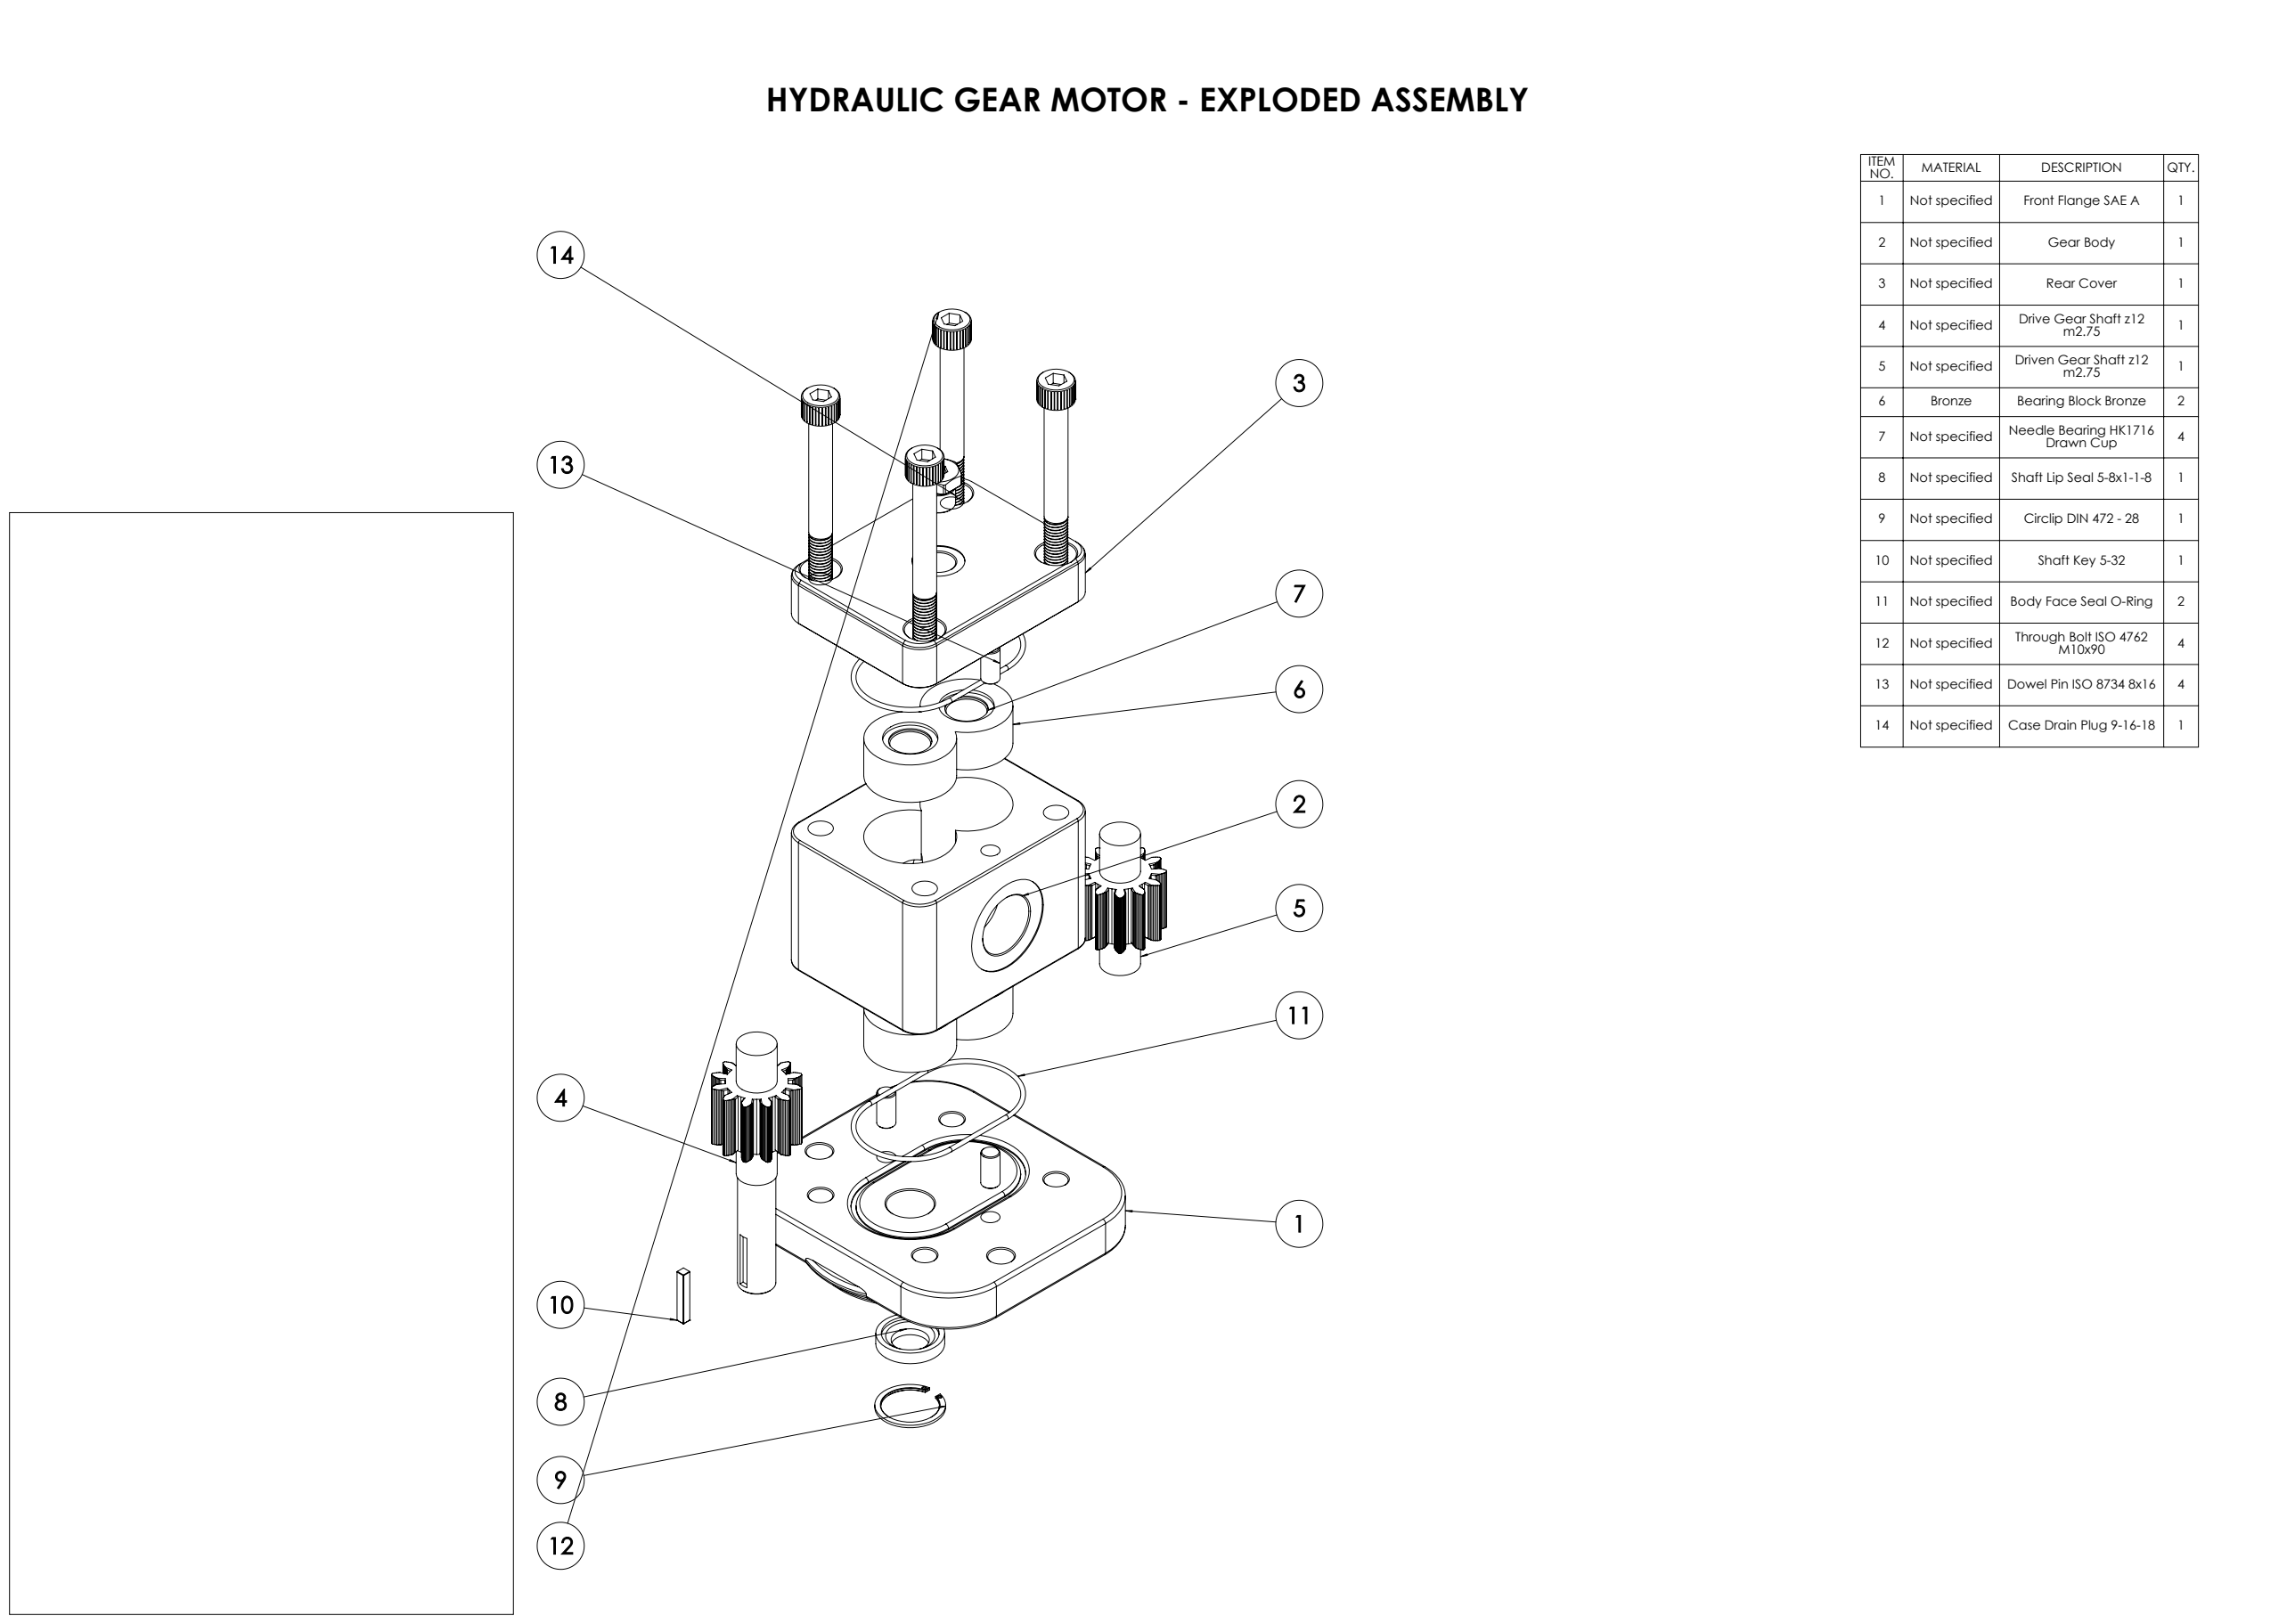
ISO-10303-21;
HEADER;
/* Generated by software containing ST-Developer
 * from STEP Tools, Inc. (www.steptools.com) 
 */

FILE_DESCRIPTION(
/* description */ (''),
/* implementation_level */ '2;1');

FILE_NAME(
/* name */ 'MAS-346',
/* time_stamp */ '2026-10-26T06:59:52-07:00',
/* author */ (''),
/* organization */ (''),
/* preprocessor_version */ 'ST-DEVELOPER v20.2',
/* originating_system */ 'Autodesk Translation Framework v15.15.0.0',
/* authorisation */ '');

FILE_SCHEMA (('AUTOMOTIVE_DESIGN { 1 0 10303 214 3 1 1 }'));
ENDSEC;

DATA;
#10=MECHANICAL_DESIGN_GEOMETRIC_PRESENTATION_REPRESENTATION('',(#164,#165,
#166,#167,#168,#169,#170,#171,#172,#173,#174,#175,#176,#177),#46395);
#11=ITEM_DEFINED_TRANSFORMATION($,$,#25107,#26908);
#12=ITEM_DEFINED_TRANSFORMATION($,$,#25445,#26909);
#13=ITEM_DEFINED_TRANSFORMATION($,$,#25562,#26910);
#14=ITEM_DEFINED_TRANSFORMATION($,$,#25703,#26911);
#15=ITEM_DEFINED_TRANSFORMATION($,$,#26063,#26912);
#16=ITEM_DEFINED_TRANSFORMATION($,$,#26410,#26913);
#17=ITEM_DEFINED_TRANSFORMATION($,$,#26410,#26914);
#18=ITEM_DEFINED_TRANSFORMATION($,$,#26435,#26915);
#19=ITEM_DEFINED_TRANSFORMATION($,$,#26457,#26916);
#20=ITEM_DEFINED_TRANSFORMATION($,$,#26494,#26917);
#21=ITEM_DEFINED_TRANSFORMATION($,$,#26513,#26918);
#22=ITEM_DEFINED_TRANSFORMATION($,$,#26513,#26919);
#23=ITEM_DEFINED_TRANSFORMATION($,$,#26528,#26920);
#24=ITEM_DEFINED_TRANSFORMATION($,$,#26580,#26921);
#25=ITEM_DEFINED_TRANSFORMATION($,$,#26580,#26922);
#26=ITEM_DEFINED_TRANSFORMATION($,$,#26580,#26923);
#27=ITEM_DEFINED_TRANSFORMATION($,$,#26580,#26924);
#28=ITEM_DEFINED_TRANSFORMATION($,$,#26605,#26925);
#29=ITEM_DEFINED_TRANSFORMATION($,$,#26605,#26926);
#30=ITEM_DEFINED_TRANSFORMATION($,$,#26605,#26927);
#31=ITEM_DEFINED_TRANSFORMATION($,$,#26605,#26928);
#32=ITEM_DEFINED_TRANSFORMATION($,$,#26898,#26929);
#33=ITEM_DEFINED_TRANSFORMATION($,$,#26898,#26930);
#34=ITEM_DEFINED_TRANSFORMATION($,$,#26898,#26931);
#35=ITEM_DEFINED_TRANSFORMATION($,$,#26898,#26932);
#36=(
REPRESENTATION_RELATIONSHIP($,$,#46456,#46455)
REPRESENTATION_RELATIONSHIP_WITH_TRANSFORMATION(#11)
SHAPE_REPRESENTATION_RELATIONSHIP()
);
#37=(
REPRESENTATION_RELATIONSHIP($,$,#46457,#46455)
REPRESENTATION_RELATIONSHIP_WITH_TRANSFORMATION(#12)
SHAPE_REPRESENTATION_RELATIONSHIP()
);
#38=(
REPRESENTATION_RELATIONSHIP($,$,#46458,#46455)
REPRESENTATION_RELATIONSHIP_WITH_TRANSFORMATION(#13)
SHAPE_REPRESENTATION_RELATIONSHIP()
);
#39=(
REPRESENTATION_RELATIONSHIP($,$,#46459,#46455)
REPRESENTATION_RELATIONSHIP_WITH_TRANSFORMATION(#14)
SHAPE_REPRESENTATION_RELATIONSHIP()
);
#40=(
REPRESENTATION_RELATIONSHIP($,$,#46460,#46455)
REPRESENTATION_RELATIONSHIP_WITH_TRANSFORMATION(#15)
SHAPE_REPRESENTATION_RELATIONSHIP()
);
#41=(
REPRESENTATION_RELATIONSHIP($,$,#46461,#46455)
REPRESENTATION_RELATIONSHIP_WITH_TRANSFORMATION(#16)
SHAPE_REPRESENTATION_RELATIONSHIP()
);
#42=(
REPRESENTATION_RELATIONSHIP($,$,#46461,#46455)
REPRESENTATION_RELATIONSHIP_WITH_TRANSFORMATION(#17)
SHAPE_REPRESENTATION_RELATIONSHIP()
);
#43=(
REPRESENTATION_RELATIONSHIP($,$,#46462,#46455)
REPRESENTATION_RELATIONSHIP_WITH_TRANSFORMATION(#18)
SHAPE_REPRESENTATION_RELATIONSHIP()
);
#44=(
REPRESENTATION_RELATIONSHIP($,$,#46463,#46455)
REPRESENTATION_RELATIONSHIP_WITH_TRANSFORMATION(#19)
SHAPE_REPRESENTATION_RELATIONSHIP()
);
#45=(
REPRESENTATION_RELATIONSHIP($,$,#46464,#46455)
REPRESENTATION_RELATIONSHIP_WITH_TRANSFORMATION(#20)
SHAPE_REPRESENTATION_RELATIONSHIP()
);
#46=(
REPRESENTATION_RELATIONSHIP($,$,#46465,#46455)
REPRESENTATION_RELATIONSHIP_WITH_TRANSFORMATION(#21)
SHAPE_REPRESENTATION_RELATIONSHIP()
);
#47=(
REPRESENTATION_RELATIONSHIP($,$,#46465,#46455)
REPRESENTATION_RELATIONSHIP_WITH_TRANSFORMATION(#22)
SHAPE_REPRESENTATION_RELATIONSHIP()
);
#48=(
REPRESENTATION_RELATIONSHIP($,$,#46466,#46455)
REPRESENTATION_RELATIONSHIP_WITH_TRANSFORMATION(#23)
SHAPE_REPRESENTATION_RELATIONSHIP()
);
#49=(
REPRESENTATION_RELATIONSHIP($,$,#46467,#46455)
REPRESENTATION_RELATIONSHIP_WITH_TRANSFORMATION(#24)
SHAPE_REPRESENTATION_RELATIONSHIP()
);
#50=(
REPRESENTATION_RELATIONSHIP($,$,#46467,#46455)
REPRESENTATION_RELATIONSHIP_WITH_TRANSFORMATION(#25)
SHAPE_REPRESENTATION_RELATIONSHIP()
);
#51=(
REPRESENTATION_RELATIONSHIP($,$,#46467,#46455)
REPRESENTATION_RELATIONSHIP_WITH_TRANSFORMATION(#26)
SHAPE_REPRESENTATION_RELATIONSHIP()
);
#52=(
REPRESENTATION_RELATIONSHIP($,$,#46467,#46455)
REPRESENTATION_RELATIONSHIP_WITH_TRANSFORMATION(#27)
SHAPE_REPRESENTATION_RELATIONSHIP()
);
#53=(
REPRESENTATION_RELATIONSHIP($,$,#46468,#46455)
REPRESENTATION_RELATIONSHIP_WITH_TRANSFORMATION(#28)
SHAPE_REPRESENTATION_RELATIONSHIP()
);
#54=(
REPRESENTATION_RELATIONSHIP($,$,#46468,#46455)
REPRESENTATION_RELATIONSHIP_WITH_TRANSFORMATION(#29)
SHAPE_REPRESENTATION_RELATIONSHIP()
);
#55=(
REPRESENTATION_RELATIONSHIP($,$,#46468,#46455)
REPRESENTATION_RELATIONSHIP_WITH_TRANSFORMATION(#30)
SHAPE_REPRESENTATION_RELATIONSHIP()
);
#56=(
REPRESENTATION_RELATIONSHIP($,$,#46468,#46455)
REPRESENTATION_RELATIONSHIP_WITH_TRANSFORMATION(#31)
SHAPE_REPRESENTATION_RELATIONSHIP()
);
#57=(
REPRESENTATION_RELATIONSHIP($,$,#46469,#46455)
REPRESENTATION_RELATIONSHIP_WITH_TRANSFORMATION(#32)
SHAPE_REPRESENTATION_RELATIONSHIP()
);
#58=(
REPRESENTATION_RELATIONSHIP($,$,#46469,#46455)
REPRESENTATION_RELATIONSHIP_WITH_TRANSFORMATION(#33)
SHAPE_REPRESENTATION_RELATIONSHIP()
);
#59=(
REPRESENTATION_RELATIONSHIP($,$,#46469,#46455)
REPRESENTATION_RELATIONSHIP_WITH_TRANSFORMATION(#34)
SHAPE_REPRESENTATION_RELATIONSHIP()
);
#60=(
REPRESENTATION_RELATIONSHIP($,$,#46469,#46455)
REPRESENTATION_RELATIONSHIP_WITH_TRANSFORMATION(#35)
SHAPE_REPRESENTATION_RELATIONSHIP()
);
#61=CONTEXT_DEPENDENT_SHAPE_REPRESENTATION(#36,#46430);
#62=CONTEXT_DEPENDENT_SHAPE_REPRESENTATION(#37,#46431);
#63=CONTEXT_DEPENDENT_SHAPE_REPRESENTATION(#38,#46432);
#64=CONTEXT_DEPENDENT_SHAPE_REPRESENTATION(#39,#46433);
#65=CONTEXT_DEPENDENT_SHAPE_REPRESENTATION(#40,#46434);
#66=CONTEXT_DEPENDENT_SHAPE_REPRESENTATION(#41,#46435);
#67=CONTEXT_DEPENDENT_SHAPE_REPRESENTATION(#42,#46436);
#68=CONTEXT_DEPENDENT_SHAPE_REPRESENTATION(#43,#46437);
#69=CONTEXT_DEPENDENT_SHAPE_REPRESENTATION(#44,#46438);
#70=CONTEXT_DEPENDENT_SHAPE_REPRESENTATION(#45,#46439);
#71=CONTEXT_DEPENDENT_SHAPE_REPRESENTATION(#46,#46440);
#72=CONTEXT_DEPENDENT_SHAPE_REPRESENTATION(#47,#46441);
#73=CONTEXT_DEPENDENT_SHAPE_REPRESENTATION(#48,#46442);
#74=CONTEXT_DEPENDENT_SHAPE_REPRESENTATION(#49,#46443);
#75=CONTEXT_DEPENDENT_SHAPE_REPRESENTATION(#50,#46444);
#76=CONTEXT_DEPENDENT_SHAPE_REPRESENTATION(#51,#46445);
#77=CONTEXT_DEPENDENT_SHAPE_REPRESENTATION(#52,#46446);
#78=CONTEXT_DEPENDENT_SHAPE_REPRESENTATION(#53,#46447);
#79=CONTEXT_DEPENDENT_SHAPE_REPRESENTATION(#54,#46448);
#80=CONTEXT_DEPENDENT_SHAPE_REPRESENTATION(#55,#46449);
#81=CONTEXT_DEPENDENT_SHAPE_REPRESENTATION(#56,#46450);
#82=CONTEXT_DEPENDENT_SHAPE_REPRESENTATION(#57,#46451);
#83=CONTEXT_DEPENDENT_SHAPE_REPRESENTATION(#58,#46452);
#84=CONTEXT_DEPENDENT_SHAPE_REPRESENTATION(#59,#46453);
#85=CONTEXT_DEPENDENT_SHAPE_REPRESENTATION(#60,#46454);
#86=NEXT_ASSEMBLY_USAGE_OCCURRENCE('01_Front_Flange_SAE_A:2',
'01_Front_Flange_SAE_A:2','01_Front_Flange_SAE_A:2',#46471,#46472,
'01_Front_Flange_SAE_A:2');
#87=NEXT_ASSEMBLY_USAGE_OCCURRENCE('02_Gear_Body:2','02_Gear_Body:2',
'02_Gear_Body:2',#46471,#46473,'02_Gear_Body:2');
#88=NEXT_ASSEMBLY_USAGE_OCCURRENCE('03_Rear_Cover:2','03_Rear_Cover:2',
'03_Rear_Cover:2',#46471,#46474,'03_Rear_Cover:2');
#89=NEXT_ASSEMBLY_USAGE_OCCURRENCE('04_Drive_Gear_Shaft_z12_m2.75:2',
'04_Drive_Gear_Shaft_z12_m2.75:2','04_Drive_Gear_Shaft_z12_m2.75:2',#46471,
#46475,'04_Drive_Gear_Shaft_z12_m2.75:2');
#90=NEXT_ASSEMBLY_USAGE_OCCURRENCE('05_Driven_Gear_Shaft_z12_m2.75:2',
'05_Driven_Gear_Shaft_z12_m2.75:2','05_Driven_Gear_Shaft_z12_m2.75:2',#46471,
#46476,'05_Driven_Gear_Shaft_z12_m2.75:2');
#91=NEXT_ASSEMBLY_USAGE_OCCURRENCE('06_Bearing_Block_Bronze:2',
'06_Bearing_Block_Bronze:2','06_Bearing_Block_Bronze:2',#46471,#46477,
'06_Bearing_Block_Bronze:2');
#92=NEXT_ASSEMBLY_USAGE_OCCURRENCE('06_Bearing_Block_Bronze:3',
'06_Bearing_Block_Bronze:3','06_Bearing_Block_Bronze:3',#46471,#46477,
'06_Bearing_Block_Bronze:3');
#93=NEXT_ASSEMBLY_USAGE_OCCURRENCE('08_Shaft_Lip_Seal_5-8x1-1-8:2',
'08_Shaft_Lip_Seal_5-8x1-1-8:2','08_Shaft_Lip_Seal_5-8x1-1-8:2',#46471,
#46478,'08_Shaft_Lip_Seal_5-8x1-1-8:2');
#94=NEXT_ASSEMBLY_USAGE_OCCURRENCE('09_Circlip_DIN_472_-_28:2',
'09_Circlip_DIN_472_-_28:2','09_Circlip_DIN_472_-_28:2',#46471,#46479,
'09_Circlip_DIN_472_-_28:2');
#95=NEXT_ASSEMBLY_USAGE_OCCURRENCE('10_Shaft_Key_5-32:2',
'10_Shaft_Key_5-32:2','10_Shaft_Key_5-32:2',#46471,#46480,
'10_Shaft_Key_5-32:2');
#96=NEXT_ASSEMBLY_USAGE_OCCURRENCE('11_Body_Face_Seal_O-Ring:2',
'11_Body_Face_Seal_O-Ring:2','11_Body_Face_Seal_O-Ring:2',#46471,#46481,
'11_Body_Face_Seal_O-Ring:2');
#97=NEXT_ASSEMBLY_USAGE_OCCURRENCE('11_Body_Face_Seal_O-Ring:3',
'11_Body_Face_Seal_O-Ring:3','11_Body_Face_Seal_O-Ring:3',#46471,#46481,
'11_Body_Face_Seal_O-Ring:3');
#98=NEXT_ASSEMBLY_USAGE_OCCURRENCE('14_Case_Drain_Plug_9-16-18:2',
'14_Case_Drain_Plug_9-16-18:2','14_Case_Drain_Plug_9-16-18:2',#46471,#46482,
'14_Case_Drain_Plug_9-16-18:2');
#99=NEXT_ASSEMBLY_USAGE_OCCURRENCE(
'07_Needle_Bearing_HK1716_Drawn_Cup:2',
'07_Needle_Bearing_HK1716_Drawn_Cup:2',
'07_Needle_Bearing_HK1716_Drawn_Cup:2',#46471,#46483,
'07_Needle_Bearing_HK1716_Drawn_Cup:2');
#100=NEXT_ASSEMBLY_USAGE_OCCURRENCE(
'07_Needle_Bearing_HK1716_Drawn_Cup:3',
'07_Needle_Bearing_HK1716_Drawn_Cup:3',
'07_Needle_Bearing_HK1716_Drawn_Cup:3',#46471,#46483,
'07_Needle_Bearing_HK1716_Drawn_Cup:3');
#101=NEXT_ASSEMBLY_USAGE_OCCURRENCE(
'07_Needle_Bearing_HK1716_Drawn_Cup:4',
'07_Needle_Bearing_HK1716_Drawn_Cup:4',
'07_Needle_Bearing_HK1716_Drawn_Cup:4',#46471,#46483,
'07_Needle_Bearing_HK1716_Drawn_Cup:4');
#102=NEXT_ASSEMBLY_USAGE_OCCURRENCE(
'07_Needle_Bearing_HK1716_Drawn_Cup:5',
'07_Needle_Bearing_HK1716_Drawn_Cup:5',
'07_Needle_Bearing_HK1716_Drawn_Cup:5',#46471,#46483,
'07_Needle_Bearing_HK1716_Drawn_Cup:5');
#103=NEXT_ASSEMBLY_USAGE_OCCURRENCE('12_Through_Bolt_ISO_4762_M10x90:2',
'12_Through_Bolt_ISO_4762_M10x90:2','12_Through_Bolt_ISO_4762_M10x90:2',
#46471,#46484,'12_Through_Bolt_ISO_4762_M10x90:2');
#104=NEXT_ASSEMBLY_USAGE_OCCURRENCE('12_Through_Bolt_ISO_4762_M10x90:3',
'12_Through_Bolt_ISO_4762_M10x90:3','12_Through_Bolt_ISO_4762_M10x90:3',
#46471,#46484,'12_Through_Bolt_ISO_4762_M10x90:3');
#105=NEXT_ASSEMBLY_USAGE_OCCURRENCE('12_Through_Bolt_ISO_4762_M10x90:4',
'12_Through_Bolt_ISO_4762_M10x90:4','12_Through_Bolt_ISO_4762_M10x90:4',
#46471,#46484,'12_Through_Bolt_ISO_4762_M10x90:4');
#106=NEXT_ASSEMBLY_USAGE_OCCURRENCE('12_Through_Bolt_ISO_4762_M10x90:5',
'12_Through_Bolt_ISO_4762_M10x90:5','12_Through_Bolt_ISO_4762_M10x90:5',
#46471,#46484,'12_Through_Bolt_ISO_4762_M10x90:5');
#107=NEXT_ASSEMBLY_USAGE_OCCURRENCE('13_Dowel_Pin_ISO_8734_8x16:2',
'13_Dowel_Pin_ISO_8734_8x16:2','13_Dowel_Pin_ISO_8734_8x16:2',#46471,#46485,
'13_Dowel_Pin_ISO_8734_8x16:2');
#108=NEXT_ASSEMBLY_USAGE_OCCURRENCE('13_Dowel_Pin_ISO_8734_8x16:3',
'13_Dowel_Pin_ISO_8734_8x16:3','13_Dowel_Pin_ISO_8734_8x16:3',#46471,#46485,
'13_Dowel_Pin_ISO_8734_8x16:3');
#109=NEXT_ASSEMBLY_USAGE_OCCURRENCE('13_Dowel_Pin_ISO_8734_8x16:4',
'13_Dowel_Pin_ISO_8734_8x16:4','13_Dowel_Pin_ISO_8734_8x16:4',#46471,#46485,
'13_Dowel_Pin_ISO_8734_8x16:4');
#110=NEXT_ASSEMBLY_USAGE_OCCURRENCE('13_Dowel_Pin_ISO_8734_8x16:5',
'13_Dowel_Pin_ISO_8734_8x16:5','13_Dowel_Pin_ISO_8734_8x16:5',#46471,#46485,
'13_Dowel_Pin_ISO_8734_8x16:5');
#111=ELLIPSE('',#26459,20.7889393668845,14.7);
#112=ELLIPSE('',#26464,20.7889393668845,14.7);
#113=ELLIPSE('',#26470,20.7889393668845,14.7);
#114=ELLIPSE('',#26474,20.7889393668845,14.7);
#115=(
BOUNDED_CURVE()
B_SPLINE_CURVE(2,(#35773,#35774,#35775),.UNSPECIFIED.,.F.,.F.)
B_SPLINE_CURVE_WITH_KNOTS((3,3),(0.,0.297909382195316),.UNSPECIFIED.)
CURVE()
GEOMETRIC_REPRESENTATION_ITEM()
RATIONAL_B_SPLINE_CURVE((1.,1.,1.))
REPRESENTATION_ITEM('')
);
#116=(
BOUNDED_CURVE()
B_SPLINE_CURVE(2,(#35780,#35781,#35782),.UNSPECIFIED.,.F.,.F.)
B_SPLINE_CURVE_WITH_KNOTS((3,3),(0.297909382195316,0.595818764390632),
 .UNSPECIFIED.)
CURVE()
GEOMETRIC_REPRESENTATION_ITEM()
RATIONAL_B_SPLINE_CURVE((1.,1.,1.))
REPRESENTATION_ITEM('')
);
#117=(
BOUNDED_CURVE()
B_SPLINE_CURVE(2,(#35788,#35789,#35790),.UNSPECIFIED.,.F.,.F.)
B_SPLINE_CURVE_WITH_KNOTS((3,3),(0.297909382195316,0.595818764390632),
 .UNSPECIFIED.)
CURVE()
GEOMETRIC_REPRESENTATION_ITEM()
RATIONAL_B_SPLINE_CURVE((1.,1.,1.))
REPRESENTATION_ITEM('')
);
#118=(
BOUNDED_CURVE()
B_SPLINE_CURVE(2,(#35792,#35793,#35794),.UNSPECIFIED.,.F.,.F.)
B_SPLINE_CURVE_WITH_KNOTS((3,3),(0.,0.297909382195316),.UNSPECIFIED.)
CURVE()
GEOMETRIC_REPRESENTATION_ITEM()
RATIONAL_B_SPLINE_CURVE((1.,1.,1.))
REPRESENTATION_ITEM('')
);
#119=(
BOUNDED_CURVE()
B_SPLINE_CURVE(2,(#35820,#35821,#35822),.UNSPECIFIED.,.F.,.F.)
B_SPLINE_CURVE_WITH_KNOTS((3,3),(0.,0.297909382195316),.UNSPECIFIED.)
CURVE()
GEOMETRIC_REPRESENTATION_ITEM()
RATIONAL_B_SPLINE_CURVE((1.,1.,1.))
REPRESENTATION_ITEM('')
);
#120=(
BOUNDED_CURVE()
B_SPLINE_CURVE(2,(#35829,#35830,#35831),.UNSPECIFIED.,.F.,.F.)
B_SPLINE_CURVE_WITH_KNOTS((3,3),(0.297909382195316,0.595818764390632),
 .UNSPECIFIED.)
CURVE()
GEOMETRIC_REPRESENTATION_ITEM()
RATIONAL_B_SPLINE_CURVE((1.,1.,1.))
REPRESENTATION_ITEM('')
);
#121=(
BOUNDED_CURVE()
B_SPLINE_CURVE(2,(#35837,#35838,#35839),.UNSPECIFIED.,.F.,.F.)
B_SPLINE_CURVE_WITH_KNOTS((3,3),(0.297909382195316,0.595818764390632),
 .UNSPECIFIED.)
CURVE()
GEOMETRIC_REPRESENTATION_ITEM()
RATIONAL_B_SPLINE_CURVE((1.,1.,1.))
REPRESENTATION_ITEM('')
);
#122=(
BOUNDED_CURVE()
B_SPLINE_CURVE(2,(#35841,#35842,#35843),.UNSPECIFIED.,.F.,.F.)
B_SPLINE_CURVE_WITH_KNOTS((3,3),(0.,0.297909382195316),.UNSPECIFIED.)
CURVE()
GEOMETRIC_REPRESENTATION_ITEM()
RATIONAL_B_SPLINE_CURVE((1.,1.,1.))
REPRESENTATION_ITEM('')
);
#123=(
BOUNDED_CURVE()
B_SPLINE_CURVE(2,(#40519,#40520,#40521),.UNSPECIFIED.,.F.,.F.)
B_SPLINE_CURVE_WITH_KNOTS((3,3),(0.179912787003236,0.267754473851814),
 .UNSPECIFIED.)
CURVE()
GEOMETRIC_REPRESENTATION_ITEM()
RATIONAL_B_SPLINE_CURVE((1.0121972483025,1.01317411304726,1.0121972483025))
REPRESENTATION_ITEM('')
);
#124=(
BOUNDED_CURVE()
B_SPLINE_CURVE(2,(#40530,#40531,#40532),.UNSPECIFIED.,.F.,.F.)
B_SPLINE_CURVE_WITH_KNOTS((3,3),(0.179912787003235,0.267754473851812),
 .UNSPECIFIED.)
CURVE()
GEOMETRIC_REPRESENTATION_ITEM()
RATIONAL_B_SPLINE_CURVE((1.01219724830249,1.01317411304725,1.01219724830249))
REPRESENTATION_ITEM('')
);
#125=(
BOUNDED_CURVE()
B_SPLINE_CURVE(2,(#40538,#40539,#40540),.UNSPECIFIED.,.F.,.F.)
B_SPLINE_CURVE_WITH_KNOTS((3,3),(0.179912787003235,0.267754473851814),
 .UNSPECIFIED.)
CURVE()
GEOMETRIC_REPRESENTATION_ITEM()
RATIONAL_B_SPLINE_CURVE((1.01219724830251,1.01317411304727,1.01219724830251))
REPRESENTATION_ITEM('')
);
#126=(
BOUNDED_CURVE()
B_SPLINE_CURVE(2,(#40549,#40550,#40551),.UNSPECIFIED.,.F.,.F.)
B_SPLINE_CURVE_WITH_KNOTS((3,3),(0.179912787003232,0.267754473851811),
 .UNSPECIFIED.)
CURVE()
GEOMETRIC_REPRESENTATION_ITEM()
RATIONAL_B_SPLINE_CURVE((1.0121972483025,1.01317411304727,1.0121972483025))
REPRESENTATION_ITEM('')
);
#127=(
BOUNDED_CURVE()
B_SPLINE_CURVE(2,(#40557,#40558,#40559),.UNSPECIFIED.,.F.,.F.)
B_SPLINE_CURVE_WITH_KNOTS((3,3),(0.179912787003235,0.267754473851813),
 .UNSPECIFIED.)
CURVE()
GEOMETRIC_REPRESENTATION_ITEM()
RATIONAL_B_SPLINE_CURVE((1.0121972483025,1.01317411304727,1.0121972483025))
REPRESENTATION_ITEM('')
);
#128=(
BOUNDED_CURVE()
B_SPLINE_CURVE(2,(#40568,#40569,#40570),.UNSPECIFIED.,.F.,.F.)
B_SPLINE_CURVE_WITH_KNOTS((3,3),(0.179912787003235,0.267754473851813),
 .UNSPECIFIED.)
CURVE()
GEOMETRIC_REPRESENTATION_ITEM()
RATIONAL_B_SPLINE_CURVE((1.0121972483025,1.01317411304726,1.0121972483025))
REPRESENTATION_ITEM('')
);
#129=(
BOUNDED_CURVE()
B_SPLINE_CURVE(2,(#40574,#40575,#40576),.UNSPECIFIED.,.F.,.F.)
B_SPLINE_CURVE_WITH_KNOTS((3,3),(0.111302637204007,1.06697395554892),
 .UNSPECIFIED.)
CURVE()
GEOMETRIC_REPRESENTATION_ITEM()
RATIONAL_B_SPLINE_CURVE((1.03421564758363,1.16578435241637,1.03421564758363))
REPRESENTATION_ITEM('')
);
#130=(
BOUNDED_CURVE()
B_SPLINE_CURVE(2,(#40579,#40580,#40581),.UNSPECIFIED.,.F.,.F.)
B_SPLINE_CURVE_WITH_KNOTS((3,3),(0.111302637204007,0.589138296376461),
 .UNSPECIFIED.)
CURVE()
GEOMETRIC_REPRESENTATION_ITEM()
RATIONAL_B_SPLINE_CURVE((1.03421564758363,1.1,1.1))
REPRESENTATION_ITEM('')
);
#131=(
BOUNDED_CURVE()
B_SPLINE_CURVE(2,(#40582,#40583,#40584),.UNSPECIFIED.,.F.,.F.)
B_SPLINE_CURVE_WITH_KNOTS((3,3),(0.589138296376461,1.06697395554892),
 .UNSPECIFIED.)
CURVE()
GEOMETRIC_REPRESENTATION_ITEM()
RATIONAL_B_SPLINE_CURVE((1.1,1.1,1.03421564758363))
REPRESENTATION_ITEM('')
);
#132=(
BOUNDED_CURVE()
B_SPLINE_CURVE(2,(#40586,#40587,#40588),.UNSPECIFIED.,.F.,.F.)
B_SPLINE_CURVE_WITH_KNOTS((3,3),(0.111302637204006,1.06697395554891),
 .UNSPECIFIED.)
CURVE()
GEOMETRIC_REPRESENTATION_ITEM()
RATIONAL_B_SPLINE_CURVE((1.03421564758363,1.16578435241637,1.03421564758363))
REPRESENTATION_ITEM('')
);
#133=(
BOUNDED_CURVE()
B_SPLINE_CURVE(2,(#40658,#40659,#40660),.UNSPECIFIED.,.F.,.F.)
B_SPLINE_CURVE_WITH_KNOTS((3,3),(0.111302637204007,1.06697395554892),
 .UNSPECIFIED.)
CURVE()
GEOMETRIC_REPRESENTATION_ITEM()
RATIONAL_B_SPLINE_CURVE((1.03421564758363,1.16578435241637,1.03421564758363))
REPRESENTATION_ITEM('')
);
#134=(
BOUNDED_CURVE()
B_SPLINE_CURVE(2,(#40661,#40662,#40663),.UNSPECIFIED.,.F.,.F.)
B_SPLINE_CURVE_WITH_KNOTS((3,3),(0.111302637204007,1.06697395554892),
 .UNSPECIFIED.)
CURVE()
GEOMETRIC_REPRESENTATION_ITEM()
RATIONAL_B_SPLINE_CURVE((1.03421564758363,1.16578435241637,1.03421564758363))
REPRESENTATION_ITEM('')
);
#135=(
BOUNDED_CURVE()
B_SPLINE_CURVE(2,(#40664,#40665,#40666),.UNSPECIFIED.,.F.,.F.)
B_SPLINE_CURVE_WITH_KNOTS((3,3),(0.111302637204006,1.06697395554892),
 .UNSPECIFIED.)
CURVE()
GEOMETRIC_REPRESENTATION_ITEM()
RATIONAL_B_SPLINE_CURVE((1.03421564758363,1.16578435241637,1.03421564758363))
REPRESENTATION_ITEM('')
);
#136=SHAPE_REPRESENTATION_RELATIONSHIP('SRR','None',#46456,#150);
#137=SHAPE_REPRESENTATION_RELATIONSHIP('SRR','None',#46457,#151);
#138=SHAPE_REPRESENTATION_RELATIONSHIP('SRR','None',#46458,#152);
#139=SHAPE_REPRESENTATION_RELATIONSHIP('SRR','None',#46459,#153);
#140=SHAPE_REPRESENTATION_RELATIONSHIP('SRR','None',#46460,#154);
#141=SHAPE_REPRESENTATION_RELATIONSHIP('SRR','None',#46461,#155);
#142=SHAPE_REPRESENTATION_RELATIONSHIP('SRR','None',#46462,#156);
#143=SHAPE_REPRESENTATION_RELATIONSHIP('SRR','None',#46463,#157);
#144=SHAPE_REPRESENTATION_RELATIONSHIP('SRR','None',#46464,#158);
#145=SHAPE_REPRESENTATION_RELATIONSHIP('SRR','None',#46465,#159);
#146=SHAPE_REPRESENTATION_RELATIONSHIP('SRR','None',#46466,#160);
#147=SHAPE_REPRESENTATION_RELATIONSHIP('SRR','None',#46467,#161);
#148=SHAPE_REPRESENTATION_RELATIONSHIP('SRR','None',#46468,#162);
#149=SHAPE_REPRESENTATION_RELATIONSHIP('SRR','None',#46469,#163);
#150=ADVANCED_BREP_SHAPE_REPRESENTATION('',(#178),#46381);
#151=ADVANCED_BREP_SHAPE_REPRESENTATION('',(#179),#46382);
#152=ADVANCED_BREP_SHAPE_REPRESENTATION('',(#180),#46383);
#153=ADVANCED_BREP_SHAPE_REPRESENTATION('',(#181),#46384);
#154=ADVANCED_BREP_SHAPE_REPRESENTATION('',(#182),#46385);
#155=ADVANCED_BREP_SHAPE_REPRESENTATION('',(#183),#46386);
#156=ADVANCED_BREP_SHAPE_REPRESENTATION('',(#184),#46387);
#157=ADVANCED_BREP_SHAPE_REPRESENTATION('',(#185),#46388);
#158=ADVANCED_BREP_SHAPE_REPRESENTATION('',(#186),#46389);
#159=ADVANCED_BREP_SHAPE_REPRESENTATION('',(#187),#46390);
#160=ADVANCED_BREP_SHAPE_REPRESENTATION('',(#188),#46391);
#161=ADVANCED_BREP_SHAPE_REPRESENTATION('',(#189),#46392);
#162=ADVANCED_BREP_SHAPE_REPRESENTATION('',(#190),#46393);
#163=ADVANCED_BREP_SHAPE_REPRESENTATION('',(#191),#46394);
#164=STYLED_ITEM('',(#46589),#178);
#165=STYLED_ITEM('',(#46575),#179);
#166=STYLED_ITEM('',(#46610),#180);
#167=STYLED_ITEM('',(#46596),#181);
#168=STYLED_ITEM('',(#46596),#182);
#169=STYLED_ITEM('',(#46596),#183);
#170=STYLED_ITEM('',(#46603),#184);
#171=STYLED_ITEM('',(#46596),#185);
#172=STYLED_ITEM('',(#46596),#186);
#173=STYLED_ITEM('',(#46603),#187);
#174=STYLED_ITEM('',(#46589),#188);
#175=STYLED_ITEM('',(#46596),#189);
#176=STYLED_ITEM('',(#46603),#190);
#177=STYLED_ITEM('',(#46596),#191);
#178=MANIFOLD_SOLID_BREP('Body1',#24937);
#179=MANIFOLD_SOLID_BREP('Body1',#24938);
#180=MANIFOLD_SOLID_BREP('Body1',#24939);
#181=MANIFOLD_SOLID_BREP('Body1',#24940);
#182=MANIFOLD_SOLID_BREP('Body1',#24941);
#183=MANIFOLD_SOLID_BREP('Body1',#24942);
#184=MANIFOLD_SOLID_BREP('Body1',#24943);
#185=MANIFOLD_SOLID_BREP('Body1',#24944);
#186=MANIFOLD_SOLID_BREP('Body1',#24945);
#187=MANIFOLD_SOLID_BREP('Body1',#24946);
#188=MANIFOLD_SOLID_BREP('Body1',#24947);
#189=MANIFOLD_SOLID_BREP('Body1',#24948);
#190=MANIFOLD_SOLID_BREP('Body1',#24949);
#191=MANIFOLD_SOLID_BREP('Body1',#24950);
#192=TOROIDAL_SURFACE('',#25235,45.5,1.5);
#193=TOROIDAL_SURFACE('',#25240,9.5,1.5);
#194=TOROIDAL_SURFACE('',#25242,45.5,1.5);
#195=TOROIDAL_SURFACE('',#25244,23.5,1.5);
#196=TOROIDAL_SURFACE('',#25255,45.5,1.5);
#197=TOROIDAL_SURFACE('',#25257,9.5,1.5);
#198=TOROIDAL_SURFACE('',#25259,23.5,1.5);
#199=TOROIDAL_SURFACE('',#25270,45.5,1.5);
#200=TOROIDAL_SURFACE('',#25271,45.5,1.5);
#201=TOROIDAL_SURFACE('',#25275,9.5,1.5);
#202=TOROIDAL_SURFACE('',#25281,9.5,1.5);
#203=TOROIDAL_SURFACE('',#25283,45.5,1.5);
#204=TOROIDAL_SURFACE('',#25285,23.5,1.5);
#205=TOROIDAL_SURFACE('',#25290,23.5,1.5);
#206=TOROIDAL_SURFACE('',#25308,26.5,1.5);
#207=TOROIDAL_SURFACE('',#25313,26.5,1.5);
#208=TOROIDAL_SURFACE('',#25318,26.5,1.5);
#209=TOROIDAL_SURFACE('',#25322,26.5,1.5);
#210=TOROIDAL_SURFACE('',#25338,45.5,1.5);
#211=TOROIDAL_SURFACE('',#25341,45.5,1.5);
#212=TOROIDAL_SURFACE('',#25348,26.5,1.5);
#213=TOROIDAL_SURFACE('',#25353,26.5,1.5);
#214=TOROIDAL_SURFACE('',#25357,26.5,1.5);
#215=TOROIDAL_SURFACE('',#25361,26.5,1.5);
#216=TOROIDAL_SURFACE('',#25365,39.78,1.5);
#217=TOROIDAL_SURFACE('',#25376,6.55,1.5);
#218=TOROIDAL_SURFACE('',#25377,39.78,1.5);
#219=TOROIDAL_SURFACE('',#25380,6.55,1.5);
#220=TOROIDAL_SURFACE('',#25381,39.78,1.5);
#221=TOROIDAL_SURFACE('',#25387,26.05,1.5);
#222=TOROIDAL_SURFACE('',#25392,26.05,1.5);
#223=TOROIDAL_SURFACE('',#25400,20.95,1.5);
#224=TOROIDAL_SURFACE('',#25405,20.95,1.5);
#225=TOROIDAL_SURFACE('',#25463,9.19999999999999,0.8);
#226=TOROIDAL_SURFACE('',#25469,9.19999999999999,0.8);
#227=TOROIDAL_SURFACE('',#25475,9.2,0.8);
#228=TOROIDAL_SURFACE('',#25481,9.19999999999999,0.8);
#229=TOROIDAL_SURFACE('',#25503,9.19999999999999,0.8);
#230=TOROIDAL_SURFACE('',#25509,9.2,0.8);
#231=TOROIDAL_SURFACE('',#25515,9.19999999999999,0.8);
#232=TOROIDAL_SURFACE('',#25520,9.19999999999999,0.8);
#233=TOROIDAL_SURFACE('',#26514,23.5,1.);
#234=TOROIDAL_SURFACE('',#26523,23.5,1.);
#235=B_SPLINE_CURVE_WITH_KNOTS('',3,(#33538,#33539,#33540,#33541,#33542,
#33543,#33544,#33545,#33546,#33547,#33548,#33549,#33550,#33551,#33552,#33553,
#33554,#33555,#33556,#33557,#33558,#33559,#33560,#33561,#33562,#33563,#33564,
#33565,#33566,#33567,#33568,#33569,#33570,#33571,#33572,#33573,#33574,#33575,
#33576,#33577,#33578,#33579,#33580,#33581,#33582,#33583,#33584,#33585,#33586,
#33587,#33588,#33589,#33590,#33591,#33592),.UNSPECIFIED.,.F.,.F.,(4,3,3,
3,3,3,3,3,3,3,3,3,3,3,3,3,3,3,4),(0.,0.0454718630237578,0.0931953780608733,
0.144039899823244,0.200168007589431,0.270586701890984,0.345292422598273,
0.401891619290293,0.45296463277568,0.503347839954974,0.552485563142507,
0.605298848839098,0.665634056697671,0.749225542523253,0.81191915689244,
0.864445081090996,0.913828865900519,0.959856605633726,1.),.UNSPECIFIED.);
#236=B_SPLINE_CURVE_WITH_KNOTS('',3,(#33594,#33595,#33596,#33597),
 .UNSPECIFIED.,.F.,.F.,(4,4),(0.,1.),.UNSPECIFIED.);
#237=B_SPLINE_CURVE_WITH_KNOTS('',3,(#33599,#33600,#33601,#33602,#33603,
#33604,#33605,#33606,#33607,#33608,#33609,#33610,#33611,#33612,#33613,#33614,
#33615,#33616,#33617,#33618,#33619,#33620,#33621,#33622,#33623,#33624,#33625,
#33626,#33627,#33628,#33629,#33630,#33631,#33632,#33633,#33634,#33635,#33636,
#33637,#33638,#33639,#33640,#33641,#33642,#33643,#33644,#33645,#33646,#33647,
#33648,#33649,#33650,#33651,#33652,#33653),.UNSPECIFIED.,.F.,.F.,(4,3,3,
3,3,3,3,3,3,3,3,3,3,3,3,3,3,3,4),(0.,0.0454743571758902,0.0932006890496271,
0.144048574957132,0.200181673047708,0.270614812390332,0.345307027643268,
0.401906381576284,0.452980318796508,0.503379519506553,0.552517196305264,
0.605331277143632,0.665671120969931,0.749253340727448,0.811940005545586,
0.864461351673364,0.913841478931635,0.959866376898225,1.),.UNSPECIFIED.);
#238=B_SPLINE_CURVE_WITH_KNOTS('',3,(#33680,#33681,#33682,#33683,#33684,
#33685),.UNSPECIFIED.,.F.,.F.,(4,1,1,4),(-1.75610615531805,-1.00348923161032,
-0.501744615805158,5.55111512312578E-16),.UNSPECIFIED.);
#239=B_SPLINE_CURVE_WITH_KNOTS('',3,(#33688,#33689,#33690,#33691,#33692,
#33693),.UNSPECIFIED.,.F.,.F.,(4,1,1,4),(-5.55111512312578E-16,0.501744615805158,
1.00348923161032,1.75610615531805),.UNSPECIFIED.);
#240=B_SPLINE_CURVE_WITH_KNOTS('',3,(#33804,#33805,#33806,#33807,#33808,
#33809,#33810),.UNSPECIFIED.,.F.,.F.,(4,1,1,1,4),(-1.75610615531805,-1.25436153951289,
-0.752616923707736,-0.501744615805158,1.11022302462516E-16),
 .UNSPECIFIED.);
#241=B_SPLINE_CURVE_WITH_KNOTS('',3,(#33811,#33812,#33813,#33814,#33815,
#33816,#33817,#33818,#33819,#33820,#33821,#33822,#33823,#33824,#33825,#33826,
#33827,#33828,#33829,#33830,#33831,#33832,#33833,#33834,#33835,#33836,#33837,
#33838,#33839,#33840,#33841,#33842,#33843,#33844,#33845,#33846,#33847,#33848,
#33849,#33850,#33851,#33852,#33853,#33854,#33855,#33856,#33857,#33858,#33859,
#33860,#33861,#33862,#33863,#33864,#33865),.UNSPECIFIED.,.F.,.F.,(4,3,3,
3,3,3,3,3,3,3,3,3,3,3,3,3,3,3,4),(0.,0.0454718630243312,0.0931953780626333,
0.144039899827111,0.200168007593285,0.270586701897688,0.345292422601244,
0.401891619293199,0.452964632777224,0.503347839955881,0.552485563143915,
0.605298848838407,0.665634056695417,0.749225542521563,0.811919156891172,
0.864445081089317,0.913828865898997,0.959856605632299,1.),.UNSPECIFIED.);
#242=B_SPLINE_CURVE_WITH_KNOTS('',3,(#33895,#33896,#33897,#33898),
 .UNSPECIFIED.,.F.,.F.,(4,4),(0.,1.),.UNSPECIFIED.);
#243=B_SPLINE_CURVE_WITH_KNOTS('',3,(#33899,#33900,#33901,#33902,#33903,
#33904,#33905,#33906,#33907,#33908,#33909,#33910,#33911,#33912,#33913,#33914,
#33915,#33916,#33917,#33918,#33919,#33920,#33921,#33922,#33923,#33924,#33925,
#33926,#33927,#33928,#33929,#33930,#33931,#33932,#33933,#33934,#33935,#33936,
#33937,#33938,#33939,#33940,#33941,#33942,#33943,#33944,#33945,#33946,#33947,
#33948,#33949,#33950,#33951,#33952,#33953),.UNSPECIFIED.,.F.,.F.,(4,3,3,
3,3,3,3,3,3,3,3,3,3,3,3,3,3,3,4),(0.,0.0454743571758495,0.0932006890494206,
0.144048574957566,0.200181673048685,0.270614812390706,0.345307027641822,
0.401906381575635,0.452980318795634,0.503379519504597,0.552517196303257,
0.605331277141522,0.665671120968433,0.749253340726325,0.811940005544743,
0.864461351672607,0.913841478930594,0.959866376897371,1.),.UNSPECIFIED.);
#244=B_SPLINE_CURVE_WITH_KNOTS('',3,(#33984,#33985,#33986,#33987,#33988,
#33989,#33990),.UNSPECIFIED.,.F.,.F.,(4,1,1,1,4),(-1.11022302462516E-16,
0.501744615805158,0.752616923707736,1.25436153951289,1.75610615531805),
 .UNSPECIFIED.);
#245=B_SPLINE_CURVE_WITH_KNOTS('',3,(#33998,#33999,#34000,#34001,#34002,
#34003,#34004,#34005,#34006,#34007,#34008,#34009,#34010,#34011),
 .UNSPECIFIED.,.F.,.F.,(4,2,2,2,2,2,4),(0.2830029806958,0.32673657269417,
0.376100941370913,0.440377410457652,0.50187293467793,0.56600596139079,0.566744275786352),
 .UNSPECIFIED.);
#246=B_SPLINE_CURVE_WITH_KNOTS('',3,(#34035,#34036,#34037,#34038,#34039,
#34040),.UNSPECIFIED.,.F.,.F.,(4,2,4),(0.457345926229208,0.511458202087047,
0.555227226239397),.UNSPECIFIED.);
#247=B_SPLINE_CURVE_WITH_KNOTS('',3,(#34044,#34045,#34046,#34047,#34048,
#34049),.UNSPECIFIED.,.F.,.F.,(4,2,4),(0.,0.0542493992714901,0.0984920623079337),
 .UNSPECIFIED.);
#248=B_SPLINE_CURVE_WITH_KNOTS('',3,(#34058,#34059,#34060,#34061,#34062,
#34063,#34064,#34065),.UNSPECIFIED.,.F.,.F.,(4,2,2,4),(0.,0.0729822624604683,
0.159547666524593,0.160512003570787),.UNSPECIFIED.);
#249=B_SPLINE_CURVE_WITH_KNOTS('',3,(#34071,#34072,#34073,#34074,#34075,
#34076,#34077,#34078),.UNSPECIFIED.,.F.,.F.,(4,2,2,4),(0.883241961717341,
0.890937005468247,0.9697019851369,1.04402990736473),.UNSPECIFIED.);
#250=B_SPLINE_CURVE_WITH_KNOTS('',3,(#34083,#34084,#34085,#34086,#34087,
#34088),.UNSPECIFIED.,.F.,.F.,(4,2,4),(-0.0984920602555225,-0.0542493992714899,
0.),.UNSPECIFIED.);
#251=B_SPLINE_CURVE_WITH_KNOTS('',3,(#34092,#34093,#34094,#34095,#34096,
#34097),.UNSPECIFIED.,.F.,.F.,(4,2,4),(0.359464626219636,0.403233650371369,
0.457345926229208),.UNSPECIFIED.);
#252=B_SPLINE_CURVE_WITH_KNOTS('',3,(#34106,#34107,#34108,#34109,#34110,
#34111,#34112,#34113),.UNSPECIFIED.,.F.,.F.,(4,2,2,4),(0.883254863276601,
0.890921572363312,0.969698219486375,1.04404196291709),.UNSPECIFIED.);
#253=B_SPLINE_CURVE_WITH_KNOTS('',3,(#34117,#34118,#34119,#34120,#34121,
#34122,#34123,#34124),.UNSPECIFIED.,.F.,.F.,(4,2,2,4),(0.,0.0729893210250683,
0.159554275962458,0.160511436887519),.UNSPECIFIED.);
#254=B_SPLINE_CURVE_WITH_KNOTS('',3,(#34130,#34131,#34132,#34133,#34134,
#34135),.UNSPECIFIED.,.F.,.F.,(4,2,4),(0.457345926229207,0.511458202087047,
0.555227226239396),.UNSPECIFIED.);
#255=B_SPLINE_CURVE_WITH_KNOTS('',3,(#34137,#34138,#34139,#34140,#34141,
#34142),.UNSPECIFIED.,.F.,.F.,(4,2,4),(0.,0.0542493992714896,0.0984920622777539),
 .UNSPECIFIED.);
#256=B_SPLINE_CURVE_WITH_KNOTS('',3,(#34146,#34147,#34148,#34149,#34150,
#34151),.UNSPECIFIED.,.F.,.F.,(4,2,4),(-0.0984920602555227,-0.0542493992714901,
0.),.UNSPECIFIED.);
#257=B_SPLINE_CURVE_WITH_KNOTS('',3,(#34153,#34154,#34155,#34156,#34157,
#34158),.UNSPECIFIED.,.F.,.F.,(4,2,4),(0.359464626219636,0.403233650371367,
0.457345926229207),.UNSPECIFIED.);
#258=B_SPLINE_CURVE_WITH_KNOTS('',3,(#34250,#34251,#34252,#34253,#34254,
#34255,#34256,#34257,#34258,#34259,#34260,#34261,#34262,#34263,#34264,#34265,
#34266,#34267,#34268,#34269,#34270,#34271,#34272,#34273,#34274,#34275,#34276,
#34277,#34278,#34279,#34280,#34281,#34282,#34283,#34284,#34285,#34286,#34287,
#34288,#34289,#34290,#34291,#34292,#34293,#34294,#34295,#34296,#34297,#34298,
#34299,#34300,#34301,#34302,#34303,#34304),.UNSPECIFIED.,.F.,.F.,(4,3,3,
3,3,3,3,3,3,3,3,3,3,3,3,3,3,3,4),(0.,0.0454718630236453,0.0931953780618335,
0.144039899826865,0.200168007592162,0.270586701896513,0.345292422605783,
0.401891619297809,0.452964632782272,0.503347839964507,0.552485563152053,
0.605298848849878,0.665634056712773,0.74922554253458,0.811919156900935,
0.864445081098314,0.913828865908445,0.959856605641832,1.),.UNSPECIFIED.);
#259=B_SPLINE_CURVE_WITH_KNOTS('',3,(#34306,#34307,#34308,#34309),
 .UNSPECIFIED.,.F.,.F.,(4,4),(0.,1.),.UNSPECIFIED.);
#260=B_SPLINE_CURVE_WITH_KNOTS('',3,(#34310,#34311,#34312,#34313,#34314,
#34315,#34316,#34317,#34318,#34319,#34320,#34321,#34322,#34323,#34324,#34325,
#34326,#34327,#34328,#34329,#34330,#34331,#34332,#34333,#34334,#34335,#34336,
#34337,#34338,#34339,#34340,#34341,#34342,#34343,#34344,#34345,#34346,#34347,
#34348,#34349,#34350,#34351,#34352,#34353,#34354,#34355,#34356,#34357,#34358,
#34359,#34360,#34361,#34362,#34363,#34364),.UNSPECIFIED.,.F.,.F.,(4,3,3,
3,3,3,3,3,3,3,3,3,3,3,3,3,3,3,4),(0.,0.0454743571759648,0.0932006890496545,
0.144048574957612,0.200181673048621,0.270614812391917,0.345307027644055,
0.401906381576845,0.452980318797118,0.503379519507497,0.552517196306345,
0.605331277144942,0.665671120971507,0.74925334072863,0.811940005546473,
0.864461351674218,0.91384147893233,0.959866376898877,1.),.UNSPECIFIED.);
#261=B_SPLINE_CURVE_WITH_KNOTS('',3,(#34390,#34391,#34392,#34393,#34394,
#34395),.UNSPECIFIED.,.F.,.F.,(4,1,1,4),(-1.75610615531806,-1.00348923161031,
-0.501744615805142,2.47024622979097E-14),.UNSPECIFIED.);
#262=B_SPLINE_CURVE_WITH_KNOTS('',3,(#34398,#34399,#34400,#34401,#34402,
#34403),.UNSPECIFIED.,.F.,.F.,(4,1,1,4),(-2.47024622979097E-14,0.501744615805142,
1.00348923161031,1.75610615531806),.UNSPECIFIED.);
#263=B_SPLINE_CURVE_WITH_KNOTS('',3,(#34414,#34415,#34416,#34417,#34418,
#34419),.UNSPECIFIED.,.F.,.F.,(4,1,1,4),(-1.75610615531805,-1.00348923161031,
-0.501744615805157,-5.27355936696957E-16),.UNSPECIFIED.);
#264=B_SPLINE_CURVE_WITH_KNOTS('',3,(#34420,#34421,#34422,#34423,#34424,
#34425,#34426,#34427,#34428,#34429,#34430,#34431,#34432,#34433,#34434,#34435,
#34436,#34437,#34438,#34439,#34440,#34441,#34442,#34443,#34444,#34445,#34446,
#34447,#34448,#34449,#34450,#34451,#34452,#34453,#34454,#34455,#34456,#34457,
#34458,#34459,#34460,#34461,#34462,#34463,#34464,#34465,#34466,#34467,#34468,
#34469,#34470,#34471,#34472,#34473,#34474),.UNSPECIFIED.,.F.,.F.,(4,3,3,
3,3,3,3,3,3,3,3,3,3,3,3,3,3,3,4),(0.,0.0454718630243914,0.0931953780626216,
0.14403989982724,0.200168007593373,0.270586701897748,0.345292422601248,
0.401891619293078,0.452964632777054,0.50334783995564,0.552485563143574,
0.605298848838025,0.665634056695,0.74922554252125,0.811919156890937,0.864445081089107,
0.91382886589878,0.959856605632085,1.),.UNSPECIFIED.);
#265=B_SPLINE_CURVE_WITH_KNOTS('',3,(#34504,#34505,#34506,#34507),
 .UNSPECIFIED.,.F.,.F.,(4,4),(0.,1.),.UNSPECIFIED.);
#266=B_SPLINE_CURVE_WITH_KNOTS('',3,(#34508,#34509,#34510,#34511,#34512,
#34513,#34514,#34515,#34516,#34517,#34518,#34519,#34520,#34521,#34522,#34523,
#34524,#34525,#34526,#34527,#34528,#34529,#34530,#34531,#34532,#34533,#34534,
#34535,#34536,#34537,#34538,#34539,#34540,#34541,#34542,#34543,#34544,#34545,
#34546,#34547,#34548,#34549,#34550,#34551,#34552,#34553,#34554,#34555,#34556,
#34557,#34558,#34559,#34560,#34561,#34562),.UNSPECIFIED.,.F.,.F.,(4,3,3,
3,3,3,3,3,3,3,3,3,3,3,3,3,3,3,4),(0.,0.0454743571761675,0.0932006890500933,
0.144048574956671,0.200181673048282,0.270614812391009,0.345307027645443,
0.401906381578876,0.452980318799016,0.503379519512151,0.552517196310239,
0.605331277149278,0.665671120975839,0.749253340731879,0.81194000554891,
0.864461351676132,0.91384147893387,0.959866376900601,1.),.UNSPECIFIED.);
#267=B_SPLINE_CURVE_WITH_KNOTS('',3,(#34589,#34590,#34591,#34592,#34593,
#34594),.UNSPECIFIED.,.F.,.F.,(4,1,1,4),(5.27355936696957E-16,0.501744615805157,
1.00348923161031,1.75610615531805),.UNSPECIFIED.);
#268=B_SPLINE_CURVE_WITH_KNOTS('',3,(#34602,#34603,#34604,#34605,#34606,
#34607,#34608,#34609,#34610,#34611,#34612,#34613,#34614,#34615),
 .UNSPECIFIED.,.F.,.F.,(4,2,2,2,2,2,4),(-0.566727656910624,-0.565965930395602,
-0.501954114034259,-0.440929548119714,-0.376258061364955,-0.326742970835578,
-0.282982965197809),.UNSPECIFIED.);
#269=B_SPLINE_CURVE_WITH_KNOTS('',3,(#34659,#34660,#34661,#34662,#34663,
#34664,#34665,#34666,#34667,#34668,#34669,#34670),.UNSPECIFIED.,.F.,.F.,
(4,2,2,2,2,4),(0.,0.0177298768866499,0.0386480203638908,0.106699501354674,
0.29072652917135,0.474753556988026),.UNSPECIFIED.);
#270=B_SPLINE_CURVE_WITH_KNOTS('',3,(#34674,#34675,#34676,#34677,#34678,
#34679,#34680,#34681,#34682,#34683,#34684,#34685),.UNSPECIFIED.,.F.,.F.,
(4,2,2,2,2,4),(1.80681462537756,1.99084165319423,2.17486868101091,2.24292016200169,
2.26383830547893,2.28156818236558),.UNSPECIFIED.);
#271=B_SPLINE_CURVE_WITH_KNOTS('',3,(#34695,#34696,#34697,#34698,#34699,
#34700,#34701,#34702,#34703,#34704,#34705,#34706,#34707,#34708),
 .UNSPECIFIED.,.F.,.F.,(4,2,2,2,2,2,4),(-1.39612360577563,-1.39460700772923,
-1.17311194871629,-0.972537848487119,-0.846807900198276,-0.765057233826425,
-0.697303504183967),.UNSPECIFIED.);
#272=B_SPLINE_CURVE_WITH_KNOTS('',3,(#34711,#34712,#34713,#34714,#34715,
#34716,#34717,#34718,#34719,#34720,#34721,#34722,#34723,#34724),
 .UNSPECIFIED.,.F.,.F.,(4,2,2,2,2,2,4),(-0.00127041341091992,0.,0.142293631997042,
0.26745747621236,0.346088913132952,0.397847011808156,0.440929147841825),
 .UNSPECIFIED.);
#273=B_SPLINE_CURVE_WITH_KNOTS('',3,(#34727,#34728,#34729,#34730,#34731,
#34732,#34733,#34734,#34735,#34736,#34737,#34738,#34739,#34740),
 .UNSPECIFIED.,.F.,.F.,(4,2,2,2,2,2,4),(-1.41597302520629,-1.41418889589625,
-1.0666111176201,-0.892135751403682,-0.801536275589833,-0.748843387075389,
-0.707094447966972),.UNSPECIFIED.);
#274=B_SPLINE_CURVE_WITH_KNOTS('',3,(#34768,#34769,#34770,#34771,#34772,
#34773,#34774,#34775,#34776,#34777,#34778,#34779,#34780,#34781),
 .UNSPECIFIED.,.F.,.F.,(4,2,2,2,2,2,4),(-1.39362312416001,-1.39199898884262,
-1.17364167365164,-0.971197013124251,-0.845224951582453,-0.76357754542349,
-0.695999491978471),.UNSPECIFIED.);
#275=B_SPLINE_CURVE_WITH_KNOTS('',3,(#34784,#34785,#34786,#34787,#34788,
#34789,#34790,#34791,#34792,#34793,#34794,#34795,#34796,#34797),
 .UNSPECIFIED.,.F.,.F.,(4,2,2,2,2,2,4),(-0.00178412931182033,0.,0.347577778842949,
0.522053145574294,0.612652621655965,0.665345510326134,0.707094449558532),
 .UNSPECIFIED.);
#276=B_SPLINE_CURVE_WITH_KNOTS('',3,(#34800,#34801,#34802,#34803,#34804,
#34805,#34806,#34807,#34808,#34809,#34810,#34811,#34812,#34813),
 .UNSPECIFIED.,.F.,.F.,(4,2,2,2,2,2,4),(-0.883128709093834,-0.881858295682913,
-0.739564663685846,-0.614400819470615,-0.535769382550153,-0.484011283875034,
-0.440929147841436),.UNSPECIFIED.);
#277=B_SPLINE_CURVE_WITH_KNOTS('',3,(#34840,#34841,#34842,#34843,#34844,
#34845,#34846,#34847,#34848,#34849,#34850,#34851,#34852,#34853),
 .UNSPECIFIED.,.F.,.F.,(4,2,2,2,2,2,4),(0.237947781581816,0.295547529372161,
0.353697178748574,0.412988302648374,0.444419571172075,0.475895563163675,
0.476565408893143),.UNSPECIFIED.);
#278=B_SPLINE_CURVE_WITH_KNOTS('',3,(#34854,#34855,#34856,#34857,#34858,
#34859,#34860,#34861,#34862,#34863,#34864,#34865,#34866,#34867),
 .UNSPECIFIED.,.F.,.F.,(4,2,2,2,2,2,4),(-0.000669845729473591,0.,0.0314759919915142,
0.0629072605151251,0.122198384414748,0.180348033790988,0.237947781581162),
 .UNSPECIFIED.);
#279=B_SPLINE_CURVE_WITH_KNOTS('',3,(#34871,#34872,#34873,#34874,#34875,
#34876,#34877,#34878,#34879,#34880,#34881,#34882,#34883,#34884),
 .UNSPECIFIED.,.F.,.F.,(4,2,2,2,2,2,4),(-0.000737243235122344,0.,0.0641388256771107,
0.1256562494953,0.189914332907335,0.239271567314492,0.283003897177937),
 .UNSPECIFIED.);
#280=B_SPLINE_CURVE_WITH_KNOTS('',3,(#34891,#34892,#34893,#34894,#34895,
#34896,#34897,#34898,#34899,#34900,#34901,#34902,#34903,#34904),
 .UNSPECIFIED.,.F.,.F.,(4,2,2,2,2,2,4),(0.440929147841474,0.484011283875067,
0.53576938255019,0.614400819470681,0.739564663685834,0.881858295682709,
0.883128709093627),.UNSPECIFIED.);
#281=B_SPLINE_CURVE_WITH_KNOTS('',3,(#34907,#34908,#34909,#34910,#34911,
#34912,#34913,#34914,#34915,#34916,#34917,#34918,#34919,#34920),
 .UNSPECIFIED.,.F.,.F.,(4,2,2,2,2,2,4),(-0.00151659805374153,0.,0.221495058999754,
0.422069157956912,0.547799105448391,0.629549771301697,0.697303500514436),
 .UNSPECIFIED.);
#282=B_SPLINE_CURVE_WITH_KNOTS('',3,(#34932,#34933,#34934,#34935,#34936,
#34937,#34938,#34939,#34940,#34941,#34942,#34943,#34944,#34945),
 .UNSPECIFIED.,.F.,.F.,(4,2,2,2,2,2,4),(-0.00127041341147968,0.,0.142293632019536,
0.267457476256502,0.346088913190727,0.397847011874902,0.44092914791602),
 .UNSPECIFIED.);
#283=B_SPLINE_CURVE_WITH_KNOTS('',3,(#34948,#34949,#34950,#34951,#34952,
#34953,#34954,#34955,#34956,#34957,#34958,#34959,#34960,#34961),
 .UNSPECIFIED.,.F.,.F.,(4,2,2,2,2,2,4),(-1.39612359503373,-1.39460699698273,
-1.17311193853035,-0.972537840238686,-0.846807893164431,-0.765057227582403,
-0.697303498594505),.UNSPECIFIED.);
#284=B_SPLINE_CURVE_WITH_KNOTS('',3,(#34965,#34966,#34967,#34968,#34969,
#34970,#34971,#34972,#34973,#34974,#34975,#34976,#34977,#34978),
 .UNSPECIFIED.,.F.,.F.,(4,2,2,2,2,2,4),(0.283003897184326,0.326736227048831,
0.37609346145714,0.440351544870681,0.501868968690292,0.566007794368658,
0.566745037603787),.UNSPECIFIED.);
#285=B_SPLINE_CURVE_WITH_KNOTS('',3,(#35089,#35090,#35091,#35092,#35093,
#35094,#35095,#35096,#35097,#35098,#35099,#35100,#35101,#35102),
 .UNSPECIFIED.,.F.,.F.,(4,2,2,2,2,2,4),(-0.000738314395613078,0.,0.0641330267183371,
0.125628550943858,0.189905020036076,0.23926938871703,0.283002980719128),
 .UNSPECIFIED.);
#286=B_SPLINE_CURVE_WITH_KNOTS('',3,(#35105,#35106,#35107,#35108,#35109,
#35110,#35111,#35112,#35113,#35114,#35115,#35116,#35117,#35118),
 .UNSPECIFIED.,.F.,.F.,(4,2,2,2,2,2,4),(-0.000761726515024963,0.,0.0640118163614976,
0.125036382276213,0.189707869031154,0.239222959560681,0.282982965198561),
 .UNSPECIFIED.);
#287=B_SPLINE_CURVE_WITH_KNOTS('',3,(#35161,#35162,#35163,#35164,#35165,
#35166,#35167,#35168),.UNSPECIFIED.,.F.,.F.,(4,2,2,4),(0.9079700629405,
0.928682763365301,1.00209186414222,1.07647666313639),.UNSPECIFIED.);
#288=B_SPLINE_CURVE_WITH_KNOTS('',3,(#35169,#35170,#35171,#35172,#35173,
#35174),.UNSPECIFIED.,.F.,.F.,(4,2,4),(0.,0.0943434934286175,0.17124459577731),
 .UNSPECIFIED.);
#289=B_SPLINE_CURVE_WITH_KNOTS('',3,(#35176,#35177,#35178,#35179,#35180,
#35181,#35182,#35183),.UNSPECIFIED.,.F.,.F.,(4,2,2,4),(0.907970062940467,
0.928682763365269,1.00209186414218,1.07647666313636),.UNSPECIFIED.);
#290=B_SPLINE_CURVE_WITH_KNOTS('',3,(#35185,#35186,#35187,#35188,#35189,
#35190),.UNSPECIFIED.,.F.,.F.,(4,2,4),(0.,0.0943434934286164,0.171244595777307),
 .UNSPECIFIED.);
#291=B_SPLINE_CURVE_WITH_KNOTS('',3,(#35527,#35528,#35529,#35530,#35531,
#35532,#35533,#35534,#35535,#35536,#35537,#35538,#35539,#35540),
 .UNSPECIFIED.,.F.,.F.,(4,2,2,2,2,2,4),(1.13912969187458,1.42739793020419,
1.87192783187775,2.07475703542203,2.27758623896631,2.45971948034335,2.64185272172039),
 .UNSPECIFIED.);
#292=B_SPLINE_CURVE_WITH_KNOTS('',3,(#35542,#35543,#35544,#35545,#35546,
#35547,#35548,#35549,#35550,#35551,#35552,#35553,#35554,#35555,#35556,#35557,
#35558,#35559,#35560,#35561,#35562,#35563,#35564,#35565,#35566,#35567),
 .UNSPECIFIED.,.F.,.F.,(4,2,2,2,2,2,2,2,2,2,2,2,4),(1.13912969187458,1.42739793020419,
1.87192783187775,2.07475703542203,2.27758623896631,2.45971948034335,2.64185272172039,
2.82398596309744,3.00611920447448,3.20894840801876,3.41177761156304,3.8563075132366,
4.14457575156621),.UNSPECIFIED.);
#293=B_SPLINE_CURVE_WITH_KNOTS('',3,(#35568,#35569,#35570,#35571,#35572,
#35573,#35574,#35575,#35576,#35577,#35578,#35579,#35580,#35581),
 .UNSPECIFIED.,.F.,.F.,(4,2,2,2,2,2,4),(2.64185272172039,2.82398596309744,
3.00611920447448,3.20894840801876,3.41177761156304,3.8563075132366,4.14457575156621),
 .UNSPECIFIED.);
#294=B_SPLINE_CURVE_WITH_KNOTS('',3,(#35587,#35588,#35589,#35590,#35591,
#35592,#35593,#35594,#35595,#35596,#35597,#35598,#35599,#35600),
 .UNSPECIFIED.,.F.,.F.,(4,2,2,2,2,2,4),(1.13912969187458,1.42739793020419,
1.87192783187775,2.07475703542203,2.27758623896631,2.45971948034335,2.64185272172039),
 .UNSPECIFIED.);
#295=B_SPLINE_CURVE_WITH_KNOTS('',3,(#35602,#35603,#35604,#35605,#35606,
#35607,#35608,#35609,#35610,#35611,#35612,#35613,#35614,#35615),
 .UNSPECIFIED.,.F.,.F.,(4,2,2,2,2,2,4),(2.64185272172039,2.82398596309744,
3.00611920447448,3.20894840801876,3.41177761156304,3.8563075132366,4.14457575156621),
 .UNSPECIFIED.);
#296=B_SPLINE_CURVE_WITH_KNOTS('',3,(#35627,#35628,#35629,#35630,#35631,
#35632,#35633,#35634,#35635,#35636,#35637,#35638,#35639,#35640,#35641,#35642,
#35643,#35644,#35645,#35646,#35647,#35648,#35649,#35650,#35651,#35652),
 .UNSPECIFIED.,.F.,.F.,(4,2,2,2,2,2,2,2,2,2,2,2,4),(1.13912969187458,1.42739793020419,
1.87192783187775,2.07475703542203,2.27758623896631,2.45971948034335,2.64185272172039,
2.82398596309744,3.00611920447448,3.20894840801876,3.41177761156304,3.8563075132366,
4.14457575156621),.UNSPECIFIED.);
#297=B_SPLINE_CURVE_WITH_KNOTS('',3,(#40254,#40255,#40256,#40257),
 .UNSPECIFIED.,.F.,.F.,(4,4),(0.,0.0322321858890298),.UNSPECIFIED.);
#298=B_SPLINE_CURVE_WITH_KNOTS('',3,(#40263,#40264,#40265,#40266),
 .UNSPECIFIED.,.F.,.F.,(4,4),(0.,0.0322321858888913),.UNSPECIFIED.);
#299=B_SPLINE_CURVE_WITH_KNOTS('',3,(#40292,#40293,#40294,#40295),
 .UNSPECIFIED.,.F.,.F.,(4,4),(0.,0.0322321858888547),.UNSPECIFIED.);
#300=B_SPLINE_CURVE_WITH_KNOTS('',3,(#40299,#40300,#40301,#40302),
 .UNSPECIFIED.,.F.,.F.,(4,4),(0.,0.0322321858887643),.UNSPECIFIED.);
#301=B_SPLINE_CURVE_WITH_KNOTS('',3,(#40735,#40736,#40737,#40738,#40739,
#40740,#40741,#40742,#40743,#40744,#40745,#40746,#40747,#40748,#40749,#40750),
 .UNSPECIFIED.,.F.,.F.,(4,3,3,3,3,4),(-4.09323272002465,-3.97204877033225,
-3.47554267404072,-2.97903657774919,-2.48253048145766,-2.06652207565088),
 .UNSPECIFIED.);
#302=B_SPLINE_CURVE_WITH_KNOTS('',3,(#40753,#40754,#40755,#40756,#40757,
#40758,#40759,#40760,#40761,#40762),.UNSPECIFIED.,.F.,.F.,(4,3,3,4),(0.,
0.496506096291522,0.993012192583062,1.11488200921577),.UNSPECIFIED.);
#303=B_SPLINE_CURVE_WITH_KNOTS('',3,(#40767,#40768,#40769,#40770,#40771,
#40772,#40773,#40774,#40775,#40776,#40777,#40778,#40779,#40780,#40781,#40782,
#40783,#40784,#40785,#40786,#40787,#40788,#40789,#40790,#40791,#40792,#40793,
#40794,#40795,#40796,#40797,#40798,#40799,#40800,#40801,#40802,#40803,#40804,
#40805,#40806),.UNSPECIFIED.,.F.,.F.,(4,3,3,3,3,3,3,3,3,3,3,3,3,4),(-10.3764180272042,
-9.93012192583063,-9.4336158295391,-8.93710973324757,-8.44060363695603,
-7.9440975406645,-7.44759144437297,-6.95108534808144,-6.45457925178991,
-5.95807315549838,-5.46156705920685,-4.96506096291531,-4.46855486662378,
-4.09323272002465),.UNSPECIFIED.);
#304=B_SPLINE_CURVE_WITH_KNOTS('',3,(#40807,#40808,#40809,#40810,#40811,
#40812,#40813,#40814,#40815,#40816,#40817,#40818,#40819,#40820,#40821,#40822,
#40823,#40824,#40825,#40826,#40827,#40828,#40829,#40830,#40831,#40832,#40833,
#40834,#40835,#40836,#40837,#40838,#40839,#40840,#40841,#40842,#40843,#40844,
#40845,#40846),.UNSPECIFIED.,.F.,.F.,(4,3,3,3,3,3,3,3,3,3,3,3,3,4),(1.11488200921577,
1.4895182888746,1.98602438516613,2.48253048145766,2.97903657774919,3.47554267404072,
3.97204877033226,4.46855486662379,4.96506096291532,5.46156705920685,5.95807315549838,
6.45457925178991,6.95108534808145,7.39806731639537),.UNSPECIFIED.);
#305=B_SPLINE_CURVE_WITH_KNOTS('',3,(#40851,#40852,#40853,#40854,#40855,
#40856,#40857,#40858,#40859,#40860,#40861,#40862,#40863,#40864,#40865,#40866,
#40867,#40868,#40869,#40870,#40871,#40872,#40873,#40874,#40875,#40876,#40877,
#40878,#40879,#40880,#40881,#40882,#40883,#40884,#40885,#40886,#40887,#40888,
#40889,#40890,#40891,#40892,#40893),.UNSPECIFIED.,.F.,.F.,(4,3,3,3,3,3,
3,3,3,3,3,3,3,3,4),(-16.6596033343838,-16.3847011776205,-15.888195081329,
-15.3916889850375,-14.8951828887459,-14.3986767924544,-13.9021706961629,
-13.4056645998713,-12.9091585035798,-12.4126524072883,-11.9161463109968,
-11.4196402147052,-10.9231341184137,-10.4266280221222,-10.3764180272042),
 .UNSPECIFIED.);
#306=B_SPLINE_CURVE_WITH_KNOTS('',3,(#40894,#40895,#40896,#40897,#40898,
#40899,#40900,#40901,#40902,#40903,#40904,#40905,#40906,#40907,#40908,#40909,
#40910,#40911,#40912,#40913,#40914,#40915,#40916,#40917,#40918,#40919,#40920,
#40921,#40922,#40923,#40924,#40925,#40926,#40927,#40928,#40929,#40930,#40931,
#40932,#40933,#40934,#40935,#40936),.UNSPECIFIED.,.F.,.F.,(4,3,3,3,3,3,
3,3,3,3,3,3,3,3,4),(7.39806731639537,7.44759144437298,7.94409754066451,
8.44060363695604,8.93710973324757,9.4336158295391,9.93012192583063,10.4266280221222,
10.9231341184137,11.4196402147052,11.9161463109967,12.4126524072883,12.9091585035798,
13.4056645998713,13.681252623575),.UNSPECIFIED.);
#307=B_SPLINE_CURVE_WITH_KNOTS('',3,(#40941,#40942,#40943,#40944,#40945,
#40946,#40947,#40948,#40949,#40950,#40951,#40952,#40953,#40954,#40955,#40956,
#40957,#40958,#40959,#40960,#40961,#40962,#40963,#40964,#40965,#40966,#40967,
#40968,#40969,#40970,#40971,#40972,#40973,#40974,#40975,#40976,#40977,#40978,
#40979,#40980,#40981,#40982,#40983),.UNSPECIFIED.,.F.,.F.,(4,3,3,3,3,3,
3,3,3,3,3,3,3,3,4),(-22.9427886415634,-22.8392804294104,-22.3427743331189,
-21.8462682368274,-21.3497621405359,-20.8532560442443,-20.3567499479528,
-19.8602438516613,-19.3637377553697,-18.8672316590782,-18.3707255627867,
-17.8742194664951,-17.3777133702036,-16.8812072739121,-16.6596033343838),
 .UNSPECIFIED.);
#308=B_SPLINE_CURVE_WITH_KNOTS('',3,(#40984,#40985,#40986,#40987,#40988,
#40989,#40990,#40991,#40992,#40993,#40994,#40995,#40996,#40997,#40998,#40999,
#41000,#41001,#41002,#41003,#41004,#41005,#41006,#41007,#41008,#41009,#41010,
#41011,#41012,#41013,#41014,#41015,#41016,#41017,#41018,#41019,#41020,#41021,
#41022,#41023,#41024,#41025,#41026),.UNSPECIFIED.,.F.,.F.,(4,3,3,3,3,3,
3,3,3,3,3,3,3,3,4),(13.681252623575,13.9021706961629,14.3986767924544,14.8951828887459,
15.3916889850375,15.888195081329,16.3847011776205,16.8812072739121,17.3777133702036,
17.8742194664951,18.3707255627867,18.8672316590782,19.3637377553697,19.8602438516613,
19.9644379307546),.UNSPECIFIED.);
#309=B_SPLINE_CURVE_WITH_KNOTS('',3,(#41031,#41032,#41033,#41034,#41035,
#41036,#41037,#41038,#41039,#41040,#41041,#41042,#41043,#41044,#41045,#41046,
#41047,#41048,#41049,#41050,#41051,#41052,#41053,#41054,#41055,#41056,#41057,
#41058,#41059,#41060,#41061,#41062,#41063,#41064,#41065,#41066,#41067,#41068,
#41069,#41070),.UNSPECIFIED.,.F.,.F.,(4,3,3,3,3,3,3,3,3,3,3,3,3,4),(-29.225973948743,
-28.7973535849088,-28.3008474886173,-27.8043413923258,-27.3078352960342,
-26.8113291997427,-26.3148231034512,-25.8183170071596,-25.3218109108681,
-24.8253048145766,-24.328798718285,-23.8322926219935,-23.335786525702,-22.9427886415634),
 .UNSPECIFIED.);
#310=B_SPLINE_CURVE_WITH_KNOTS('',3,(#41071,#41072,#41073,#41074,#41075,
#41076,#41077,#41078,#41079,#41080,#41081,#41082,#41083,#41084,#41085,#41086,
#41087,#41088,#41089,#41090,#41091,#41092,#41093,#41094,#41095,#41096,#41097,
#41098,#41099,#41100,#41101,#41102,#41103,#41104,#41105,#41106,#41107,#41108,
#41109,#41110),.UNSPECIFIED.,.F.,.F.,(4,3,3,3,3,3,3,3,3,3,3,3,3,4),(19.9644379307546,
20.3567499479528,20.8532560442443,21.3497621405358,21.8462682368274,22.3427743331189,
22.8392804294104,23.335786525702,23.8322926219935,24.328798718285,24.8253048145766,
25.3218109108681,25.8183170071596,26.2476232379342),.UNSPECIFIED.);
#311=B_SPLINE_CURVE_WITH_KNOTS('',3,(#41115,#41116,#41117,#41118,#41119,
#41120,#41121,#41122,#41123,#41124,#41125,#41126,#41127,#41128,#41129,#41130,
#41131,#41132,#41133,#41134,#41135,#41136,#41137,#41138,#41139,#41140,#41141,
#41142,#41143,#41144,#41145,#41146,#41147,#41148,#41149,#41150,#41151,#41152,
#41153,#41154,#41155,#41156,#41157),.UNSPECIFIED.,.F.,.F.,(4,3,3,3,3,3,
3,3,3,3,3,3,3,3,4),(-35.5091592559226,-35.2519328366987,-34.7554267404072,
-34.2589206441157,-33.7624145478241,-33.2659084515326,-32.7694023552411,
-32.2728962589495,-31.776390162658,-31.2798840663665,-30.7833779700749,
-30.2868718737834,-29.7903657774919,-29.2938596812004,-29.225973948743),
 .UNSPECIFIED.);
#312=B_SPLINE_CURVE_WITH_KNOTS('',3,(#41158,#41159,#41160,#41161,#41162,
#41163,#41164,#41165,#41166,#41167,#41168,#41169,#41170,#41171,#41172,#41173,
#41174,#41175,#41176,#41177,#41178,#41179,#41180,#41181,#41182,#41183,#41184,
#41185,#41186,#41187,#41188,#41189,#41190,#41191,#41192,#41193,#41194,#41195,
#41196,#41197,#41198,#41199,#41200),.UNSPECIFIED.,.F.,.F.,(4,3,3,3,3,3,
3,3,3,3,3,3,3,3,4),(26.2476232379342,26.3148231034511,26.8113291997427,
27.3078352960342,27.8043413923257,28.3008474886173,28.7973535849088,29.2938596812003,
29.7903657774919,30.2868718737834,30.783377970075,31.2798840663665,31.776390162658,
32.2728962589496,32.5308085451137),.UNSPECIFIED.);
#313=B_SPLINE_CURVE_WITH_KNOTS('',3,(#41205,#41206,#41207,#41208,#41209,
#41210,#41211,#41212,#41213,#41214,#41215,#41216,#41217,#41218,#41219,#41220,
#41221,#41222,#41223,#41224,#41225,#41226,#41227,#41228,#41229,#41230,#41231,
#41232,#41233,#41234,#41235,#41236,#41237,#41238,#41239,#41240,#41241,#41242,
#41243,#41244,#41245,#41246,#41247),.UNSPECIFIED.,.F.,.F.,(4,3,3,3,3,3,
3,3,3,3,3,3,3,3,4),(-41.7923445631022,-41.7065120884886,-41.2100059921971,
-40.7134998959056,-40.216993799614,-39.7204877033225,-39.223981607031,-38.7274755107394,
-38.2309694144479,-37.7344633181564,-37.2379572218649,-36.7414511255733,
-36.2449450292818,-35.7484389329903,-35.5091592559226),.UNSPECIFIED.);
#314=B_SPLINE_CURVE_WITH_KNOTS('',3,(#41248,#41249,#41250,#41251,#41252,
#41253,#41254,#41255,#41256,#41257,#41258,#41259,#41260,#41261,#41262,#41263,
#41264,#41265,#41266,#41267,#41268,#41269,#41270,#41271,#41272,#41273,#41274,
#41275,#41276,#41277,#41278,#41279,#41280,#41281,#41282,#41283,#41284,#41285,
#41286,#41287,#41288,#41289,#41290),.UNSPECIFIED.,.F.,.F.,(4,3,3,3,3,3,
3,3,3,3,3,3,3,3,4),(32.5308085451137,32.7694023552411,33.2659084515326,
33.7624145478241,34.2589206441157,34.7554267404072,35.2519328366987,35.7484389329903,
36.2449450292818,36.7414511255733,37.2379572218648,37.7344633181564,38.2309694144479,
38.7274755107394,38.8139938522933),.UNSPECIFIED.);
#315=B_SPLINE_CURVE_WITH_KNOTS('',3,(#41295,#41296,#41297,#41298,#41299,
#41300,#41301,#41302,#41303,#41304,#41305,#41306,#41307,#41308,#41309,#41310,
#41311,#41312,#41313,#41314,#41315,#41316,#41317,#41318,#41319,#41320,#41321,
#41322,#41323,#41324,#41325,#41326,#41327,#41328,#41329,#41330,#41331,#41332,
#41333,#41334),.UNSPECIFIED.,.F.,.F.,(4,3,3,3,3,3,3,3,3,3,3,3,3,4),(-48.0755298702818,
-47.664585243987,-47.1680791476955,-46.6715730514039,-46.1750669551124,
-45.6785608588209,-45.1820547625294,-44.6855486662378,-44.1890425699463,
-43.6925364736548,-43.1960303773632,-42.6995242810717,-42.2030181847802,
-41.7923445631022),.UNSPECIFIED.);
#316=B_SPLINE_CURVE_WITH_KNOTS('',3,(#41335,#41336,#41337,#41338,#41339,
#41340,#41341,#41342,#41343,#41344,#41345,#41346,#41347,#41348,#41349,#41350,
#41351,#41352,#41353,#41354,#41355,#41356,#41357,#41358,#41359,#41360,#41361,
#41362,#41363,#41364,#41365,#41366,#41367,#41368,#41369,#41370,#41371,#41372,
#41373,#41374),.UNSPECIFIED.,.F.,.F.,(4,3,3,3,3,3,3,3,3,3,3,3,3,4),(38.8139938522933,
39.223981607031,39.7204877033225,40.216993799614,40.7134998959056,41.2100059921971,
41.7065120884886,42.2030181847802,42.6995242810717,43.1960303773632,43.6925364736548,
44.1890425699463,44.6855486662378,45.0971791594729),.UNSPECIFIED.);
#317=B_SPLINE_CURVE_WITH_KNOTS('',3,(#41379,#41380,#41381,#41382,#41383,
#41384,#41385,#41386,#41387,#41388,#41389,#41390,#41391,#41392,#41393,#41394,
#41395,#41396,#41397,#41398,#41399,#41400,#41401,#41402,#41403,#41404,#41405,
#41406,#41407,#41408,#41409,#41410,#41411,#41412,#41413,#41414,#41415,#41416,
#41417,#41418,#41419,#41420,#41421),.UNSPECIFIED.,.F.,.F.,(4,3,3,3,3,3,
3,3,3,3,3,3,3,3,4),(-54.3587151774614,-54.1191644957769,-53.6226583994854,
-53.1261523031939,-52.6296462069023,-52.1331401106108,-51.6366340143193,
-51.1401279180277,-50.6436218217362,-50.1471157254447,-49.6506096291531,
-49.1541035328616,-48.6575974365701,-48.1610913402785,-48.0755298702818),
 .UNSPECIFIED.);
#318=B_SPLINE_CURVE_WITH_KNOTS('',3,(#41422,#41423,#41424,#41425,#41426,
#41427,#41428,#41429,#41430,#41431,#41432,#41433,#41434,#41435,#41436,#41437,
#41438,#41439,#41440,#41441,#41442,#41443,#41444,#41445,#41446,#41447,#41448,
#41449,#41450,#41451,#41452,#41453,#41454,#41455,#41456,#41457,#41458,#41459,
#41460,#41461,#41462,#41463,#41464),.UNSPECIFIED.,.F.,.F.,(4,3,3,3,3,3,
3,3,3,3,3,3,3,3,4),(45.0971791594729,45.1820547625293,45.6785608588209,
46.1750669551124,46.6715730514039,47.1680791476955,47.664585243987,48.1610913402785,
48.6575974365701,49.1541035328616,49.6506096291531,50.1471157254447,50.6436218217362,
51.1401279180277,51.3803644666525),.UNSPECIFIED.);
#319=B_SPLINE_CURVE_WITH_KNOTS('',3,(#41469,#41470,#41471,#41472,#41473,
#41474,#41475,#41476,#41477,#41478,#41479,#41480,#41481,#41482,#41483,#41484,
#41485,#41486,#41487,#41488,#41489,#41490,#41491,#41492,#41493,#41494,#41495,
#41496,#41497,#41498,#41499,#41500,#41501,#41502),.UNSPECIFIED.,.F.,.F.,
(4,3,3,3,3,3,3,3,3,3,3,4),(-60.641900484641,-60.5737437475668,-59.5807315549838,
-58.5877193624007,-57.5947071698176,-57.0982010735261,-56.6016949772346,
-56.1051888809431,-55.6086827846515,-55.11217668836,-54.6156705920684,-54.3587151774614),
 .UNSPECIFIED.);
#320=B_SPLINE_CURVE_WITH_KNOTS('',3,(#41503,#41504,#41505,#41506,#41507,
#41508,#41509,#41510,#41511,#41512,#41513,#41514,#41515,#41516,#41517,#41518,
#41519,#41520,#41521,#41522,#41523,#41524,#41525,#41526,#41527,#41528,#41529,
#41530,#41531,#41532,#41533,#41534,#41535,#41536,#41537,#41538,#41539,#41540,
#41541,#41542),.UNSPECIFIED.,.F.,.F.,(4,3,3,3,3,3,3,3,3,3,3,3,3,4),(51.3803644666525,
51.6366340143193,52.1331401106108,52.6296462069023,53.1261523031939,53.6226583994854,
54.1191644957769,54.6156705920685,55.11217668836,55.6086827846515,56.1051888809431,
56.6016949772346,57.5947071698176,57.6635497738321),.UNSPECIFIED.);
#321=B_SPLINE_CURVE_WITH_KNOTS('',3,(#41547,#41548,#41549,#41550,#41551,
#41552,#41553,#41554,#41555,#41556,#41557,#41558,#41559,#41560,#41561,#41562,
#41563,#41564,#41565,#41566,#41567,#41568),.UNSPECIFIED.,.F.,.F.,(4,3,3,
3,3,3,3,4),(-66.9250857918206,-66.5318169030652,-65.5388047104821,-64.5457925178991,
-63.552780325316,-62.5597681327329,-61.5667559401499,-60.641900484641),
 .UNSPECIFIED.);
#322=B_SPLINE_CURVE_WITH_KNOTS('',3,(#41569,#41570,#41571,#41572,#41573,
#41574,#41575,#41576,#41577,#41578,#41579,#41580,#41581,#41582,#41583,#41584,
#41585,#41586,#41587,#41588,#41589,#41590),.UNSPECIFIED.,.F.,.F.,(4,3,3,
3,3,3,3,4),(57.6635497738321,58.5877193624007,59.5807315549838,60.5737437475668,
61.5667559401499,62.5597681327329,63.552780325316,63.9467350810117),
 .UNSPECIFIED.);
#323=B_SPLINE_CURVE_WITH_KNOTS('',3,(#41595,#41596,#41597,#41598,#41599,
#41600,#41601,#41602,#41603,#41604,#41605,#41606,#41607,#41608,#41609,#41610,
#41611,#41612,#41613,#41614,#41615,#41616,#41617,#41618,#41619,#41620,#41621,
#41622),.UNSPECIFIED.,.F.,.F.,(4,3,3,3,3,3,3,3,3,4),(-73.2082710990002,
-72.9863961548551,-72.4898900585636,-71.993383962272,-71.4968778659805,
-70.5038656733974,-69.5108534808144,-68.5178412882313,-67.5248290956483,
-66.9250857918206),.UNSPECIFIED.);
#324=B_SPLINE_CURVE_WITH_KNOTS('',3,(#41623,#41624,#41625,#41626,#41627,
#41628,#41629,#41630,#41631,#41632,#41633,#41634,#41635,#41636,#41637,#41638,
#41639,#41640,#41641,#41642,#41643,#41644),.UNSPECIFIED.,.F.,.F.,(4,3,3,
3,3,3,3,4),(63.9467350810117,64.5457925178991,65.5388047104821,66.5318169030652,
67.5248290956483,68.5178412882313,69.5108534808144,70.2299203881913),
 .UNSPECIFIED.);
#325=B_SPLINE_CURVE_WITH_KNOTS('',3,(#41649,#41650,#41651,#41652,#41653,
#41654,#41655,#41656,#41657,#41658,#41659,#41660,#41661,#41662,#41663,#41664,
#41665,#41666,#41667,#41668,#41669,#41670,#41671,#41672,#41673,#41674,#41675,
#41676,#41677,#41678,#41679,#41680,#41681,#41682,#41683,#41684,#41685,#41686,
#41687,#41688,#41689,#41690,#41691),.UNSPECIFIED.,.F.,.F.,(4,3,3,3,3,3,
3,3,3,3,3,3,3,3,4),(-79.4914564061798,-79.440975406645,-78.9444693103535,
-78.4479632140619,-77.9514571177704,-77.4549510214789,-76.9584449251874,
-76.4619388288958,-75.9654327326043,-75.4689266363128,-74.9724205400212,
-74.4759144437297,-73.9794083474382,-73.4829022511466,-73.2082710990002),
 .UNSPECIFIED.);
#326=B_SPLINE_CURVE_WITH_KNOTS('',3,(#41692,#41693,#41694,#41695,#41696,
#41697,#41698,#41699,#41700,#41701,#41702,#41703,#41704,#41705,#41706,#41707,
#41708,#41709,#41710,#41711,#41712,#41713,#41714,#41715,#41716,#41717,#41718,
#41719,#41720,#41721,#41722,#41723,#41724,#41725,#41726,#41727,#41728),
 .UNSPECIFIED.,.F.,.F.,(4,3,3,3,3,3,3,3,3,3,3,3,4),(70.2299203881913,70.5038656733975,
71.4968778659805,72.4898900585636,72.9863961548551,73.4829022511466,73.9794083474382,
74.4759144437297,74.9724205400212,75.4689266363127,75.9654327326043,76.4619388288958,
76.5131056953709),.UNSPECIFIED.);
#327=B_SPLINE_CURVE_WITH_KNOTS('',3,(#41733,#41734,#41735,#41736,#41737,
#41738,#41739,#41740,#41741,#41742,#41743,#41744,#41745,#41746,#41747,#41748,
#41749,#41750,#41751,#41752,#41753,#41754,#41755,#41756,#41757,#41758,#41759,
#41760,#41761,#41762,#41763,#41764,#41765,#41766,#41767,#41768,#41769,#41770,
#41771,#41772),.UNSPECIFIED.,.F.,.F.,(4,3,3,3,3,3,3,3,3,3,3,3,3,4),(-85.7746417133594,
-85.3990485621434,-84.9025424658519,-84.4060363695603,-83.9095302732688,
-83.4130241769773,-82.9165180806857,-82.4200119843942,-81.9235058881027,
-81.4269997918111,-80.9304936955196,-80.4339875992281,-79.9374815029365,
-79.4914564061798),.UNSPECIFIED.);
#328=B_SPLINE_CURVE_WITH_KNOTS('',3,(#41773,#41774,#41775,#41776,#41777,
#41778,#41779,#41780,#41781,#41782,#41783,#41784,#41785,#41786,#41787,#41788,
#41789,#41790,#41791,#41792,#41793,#41794,#41795,#41796,#41797,#41798,#41799,
#41800,#41801,#41802,#41803,#41804,#41805,#41806,#41807,#41808,#41809,#41810,
#41811,#41812),.UNSPECIFIED.,.F.,.F.,(4,3,3,3,3,3,3,3,3,3,3,3,3,4),(76.5131056953709,
76.9584449251873,77.4549510214789,77.9514571177704,78.4479632140619,78.9444693103535,
79.440975406645,79.9374815029365,80.4339875992281,80.9304936955196,81.4269997918111,
81.9235058881027,82.4200119843942,82.7962910025505),.UNSPECIFIED.);
#329=B_SPLINE_CURVE_WITH_KNOTS('',3,(#41817,#41818,#41819,#41820,#41821,
#41822,#41823,#41824,#41825,#41826,#41827,#41828,#41829,#41830,#41831,#41832,
#41833,#41834,#41835,#41836,#41837,#41838,#41839,#41840,#41841,#41842,#41843,
#41844,#41845,#41846,#41847,#41848,#41849,#41850,#41851,#41852,#41853,#41854,
#41855,#41856,#41857,#41858,#41859),.UNSPECIFIED.,.F.,.F.,(4,3,3,3,3,3,
3,3,3,3,3,3,3,3,4),(-92.0578270205389,-91.8536278139333,-91.3571217176418,
-90.8606156213502,-90.3641095250587,-89.8676034287672,-89.3710973324757,
-88.8745912361841,-88.3780851398926,-87.8815790436011,-87.3850729473095,
-86.888566851018,-86.3920607547265,-85.8955546584349,-85.7746417133594),
 .UNSPECIFIED.);
#330=B_SPLINE_CURVE_WITH_KNOTS('',3,(#41860,#41861,#41862,#41863,#41864,
#41865,#41866,#41867,#41868,#41869,#41870,#41871,#41872,#41873,#41874,#41875,
#41876,#41877,#41878,#41879,#41880,#41881,#41882,#41883,#41884,#41885,#41886,
#41887,#41888,#41889,#41890,#41891,#41892,#41893,#41894,#41895,#41896,#41897,
#41898,#41899,#41900,#41901,#41902),.UNSPECIFIED.,.F.,.F.,(4,3,3,3,3,3,
3,3,3,3,3,3,3,3,4),(82.7962910025505,82.9165180806857,83.4130241769772,
83.9095302732688,84.4060363695603,84.9025424658518,85.3990485621434,85.8955546584349,
86.3920607547264,86.888566851018,87.3850729473095,87.881579043601,88.3780851398926,
88.8745912361841,89.0794763097301),.UNSPECIFIED.);
#331=B_SPLINE_CURVE_WITH_KNOTS('',3,(#41907,#41908,#41909,#41910,#41911,
#41912,#41913,#41914,#41915,#41916,#41917,#41918,#41919,#41920,#41921,#41922,
#41923,#41924,#41925,#41926,#41927,#41928,#41929,#41930,#41931,#41932,#41933,
#41934,#41935,#41936,#41937,#41938,#41939,#41940,#41941,#41942,#41943,#41944,
#41945,#41946,#41947,#41948,#41949),.UNSPECIFIED.,.F.,.F.,(4,3,3,3,3,3,
3,3,3,3,3,3,3,3,4),(-98.3410123277185,-98.3082070657232,-97.8117009694317,
-97.3151948731401,-96.8186887768486,-96.3221826805571,-95.8256765842656,
-95.329170487974,-94.8326643916825,-94.336158295391,-93.8396521990994,-93.3431461028079,
-92.8466400065164,-92.3501339102248,-92.0578270205389),.UNSPECIFIED.);
#332=B_SPLINE_CURVE_WITH_KNOTS('',3,(#41950,#41951,#41952,#41953,#41954,
#41955,#41956,#41957,#41958,#41959,#41960,#41961,#41962,#41963,#41964,#41965,
#41966,#41967,#41968,#41969,#41970,#41971,#41972,#41973,#41974,#41975,#41976,
#41977,#41978,#41979,#41980,#41981,#41982,#41983,#41984,#41985,#41986,#41987,
#41988,#41989,#41990,#41991,#41992),.UNSPECIFIED.,.F.,.F.,(4,3,3,3,3,3,
3,3,3,3,3,3,3,3,4),(89.0794763097301,89.3710973324756,89.8676034287672,
90.3641095250587,90.8606156213502,91.3571217176417,91.8536278139333,92.3501339102248,
92.8466400065163,93.3431461028079,93.8396521990994,94.3361582953909,94.8326643916825,
95.329170487974,95.3626616169096),.UNSPECIFIED.);
#333=B_SPLINE_CURVE_WITH_KNOTS('',3,(#41997,#41998,#41999,#42000,#42001,
#42002,#42003,#42004,#42005,#42006,#42007,#42008,#42009,#42010,#42011,#42012,
#42013,#42014,#42015,#42016,#42017,#42018,#42019,#42020,#42021,#42022,#42023,
#42024,#42025,#42026,#42027,#42028,#42029,#42030,#42031,#42032,#42033,#42034,
#42035,#42036),.UNSPECIFIED.,.F.,.F.,(4,3,3,3,3,3,3,3,3,3,3,3,3,4),(-104.624197634898,
-104.266280221222,-103.76977412493,-103.273268028639,-102.776761932347,
-102.280255836055,-101.783749739764,-101.287243643472,-100.790737547181,
-100.294231450889,-99.7977253545978,-99.3012192583063,-98.8047131620147,
-98.3410123277185),.UNSPECIFIED.);
#334=B_SPLINE_CURVE_WITH_KNOTS('',3,(#42037,#42038,#42039,#42040,#42041,
#42042,#42043,#42044,#42045,#42046,#42047,#42048,#42049,#42050,#42051,#42052,
#42053,#42054,#42055,#42056,#42057,#42058,#42059,#42060,#42061,#42062,#42063,
#42064,#42065,#42066,#42067,#42068,#42069,#42070,#42071,#42072,#42073,#42074,
#42075,#42076),.UNSPECIFIED.,.F.,.F.,(4,3,3,3,3,3,3,3,3,3,3,3,3,4),(95.3626616169096,
95.8256765842655,96.3221826805571,96.8186887768486,97.3151948731401,97.8117009694316,
98.3082070657232,98.8047131620147,99.3012192583062,99.7977253545978,100.294231450889,
100.790737547181,101.287243643472,101.645846924089),.UNSPECIFIED.);
#335=B_SPLINE_CURVE_WITH_KNOTS('',3,(#42081,#42082,#42083,#42084,#42085,
#42086,#42087,#42088,#42089,#42090,#42091,#42092,#42093,#42094,#42095,#42096,
#42097,#42098,#42099,#42100,#42101,#42102,#42103,#42104,#42105,#42106,#42107,
#42108,#42109,#42110,#42111,#42112,#42113,#42114,#42115,#42116,#42117,#42118,
#42119,#42120,#42121,#42122,#42123),.UNSPECIFIED.,.F.,.F.,(4,3,3,3,3,3,
3,3,3,3,3,3,3,3,4),(-110.907382942078,-110.720859473011,-110.22435337672,
-109.727847280428,-109.231341184137,-108.734835087845,-108.238328991554,
-107.741822895262,-107.245316798971,-106.748810702679,-106.252304606388,
-105.755798510096,-105.259292413805,-104.762786317513,-104.624197634898),
 .UNSPECIFIED.);
#336=B_SPLINE_CURVE_WITH_KNOTS('',3,(#42124,#42125,#42126,#42127,#42128,
#42129,#42130,#42131,#42132,#42133,#42134,#42135,#42136,#42137,#42138,#42139,
#42140,#42141,#42142,#42143,#42144,#42145,#42146,#42147,#42148,#42149,#42150,
#42151,#42152,#42153,#42154,#42155,#42156,#42157,#42158,#42159,#42160,#42161,
#42162,#42163,#42164,#42165,#42166),.UNSPECIFIED.,.F.,.F.,(4,3,3,3,3,3,
3,3,3,3,3,3,3,3,4),(101.645846924089,101.783749739764,102.280255836055,
102.776761932347,103.273268028638,103.76977412493,104.266280221222,104.762786317513,
105.259292413805,105.755798510096,106.252304606388,106.748810702679,107.245316798971,
107.741822895262,107.929032231269),.UNSPECIFIED.);
#337=B_SPLINE_CURVE_WITH_KNOTS('',3,(#42171,#42172,#42173,#42174,#42175,
#42176,#42177,#42178,#42179,#42180,#42181,#42182,#42183,#42184,#42185,#42186,
#42187,#42188,#42189,#42190,#42191,#42192,#42193,#42194,#42195,#42196,#42197,
#42198,#42199,#42200,#42201,#42202,#42203,#42204,#42205,#42206,#42207,#42208,
#42209,#42210,#42211,#42212,#42213),.UNSPECIFIED.,.F.,.F.,(4,3,3,3,3,3,
3,3,3,3,3,3,3,3,4),(-117.190568249257,-117.175438724801,-116.67893262851,
-116.182426532218,-115.685920435927,-115.189414339635,-114.692908243344,
-114.196402147052,-113.699896050761,-113.203389954469,-112.706883858178,
-112.210377761886,-111.713871665595,-111.217365569303,-110.907382942078),
 .UNSPECIFIED.);
#338=B_SPLINE_CURVE_WITH_KNOTS('',3,(#42214,#42215,#42216,#42217,#42218,
#42219,#42220,#42221,#42222,#42223,#42224,#42225,#42226,#42227,#42228,#42229,
#42230,#42231,#42232,#42233,#42234,#42235,#42236,#42237,#42238,#42239,#42240,
#42241,#42242,#42243,#42244,#42245,#42246,#42247,#42248,#42249,#42250,#42251,
#42252,#42253,#42254,#42255,#42256),.UNSPECIFIED.,.F.,.F.,(4,3,3,3,3,3,
3,3,3,3,3,3,3,3,4),(107.929032231269,108.238328991554,108.734835087845,
109.231341184137,109.727847280428,110.22435337672,110.720859473011,111.217365569303,
111.713871665595,112.210377761886,112.706883858178,113.203389954469,113.699896050761,
114.196402147052,114.212217538448),.UNSPECIFIED.);
#339=B_SPLINE_CURVE_WITH_KNOTS('',3,(#42261,#42262,#42263,#42264,#42265,
#42266,#42267,#42268,#42269,#42270,#42271,#42272,#42273,#42274,#42275,#42276,
#42277,#42278,#42279,#42280,#42281,#42282,#42283,#42284,#42285,#42286,#42287,
#42288,#42289,#42290,#42291,#42292,#42293,#42294,#42295,#42296,#42297,#42298,
#42299,#42300),.UNSPECIFIED.,.F.,.F.,(4,3,3,3,3,3,3,3,3,3,3,3,3,4),(-123.473753556437,
-123.1335118803,-122.637005784008,-122.140499687717,-121.643993591425,-121.147487495134,
-120.650981398842,-120.154475302551,-119.657969206259,-119.161463109968,
-118.664957013676,-118.168450917384,-117.671944821093,-117.190568249257),
 .UNSPECIFIED.);
#340=B_SPLINE_CURVE_WITH_KNOTS('',3,(#42301,#42302,#42303,#42304,#42305,
#42306,#42307,#42308,#42309,#42310,#42311,#42312,#42313,#42314,#42315,#42316,
#42317,#42318,#42319,#42320,#42321,#42322,#42323,#42324,#42325,#42326,#42327,
#42328,#42329,#42330,#42331,#42332,#42333,#42334,#42335,#42336,#42337,#42338,
#42339,#42340),.UNSPECIFIED.,.F.,.F.,(4,3,3,3,3,3,3,3,3,3,3,3,3,4),(114.212217538448,
114.692908243344,115.189414339635,115.685920435927,116.182426532218,116.67893262851,
117.175438724801,117.671944821093,118.168450917384,118.664957013676,119.161463109967,
119.657969206259,120.154475302551,120.495402845628),.UNSPECIFIED.);
#341=B_SPLINE_CURVE_WITH_KNOTS('',3,(#42347,#42348,#42349,#42350,#42351,
#42352,#42353,#42354,#42355,#42356,#42357,#42358,#42359,#42360,#42361,#42362,
#42363,#42364,#42365,#42366,#42367,#42368,#42369,#42370,#42371,#42372,#42373,
#42374,#42375,#42376,#42377,#42378,#42379,#42380,#42381,#42382,#42383),
 .UNSPECIFIED.,.F.,.F.,(4,3,3,3,3,3,3,3,3,3,3,3,4),(-129.091585035798,-128.595078939507,
-128.098572843215,-127.602066746924,-127.105560650632,-126.60905455434,
-126.112548458049,-125.616042361757,-125.119536265466,-124.623030169174,
-124.126524072883,-123.630017976591,-123.473753556437),.UNSPECIFIED.);
#342=B_SPLINE_CURVE_WITH_KNOTS('',3,(#42384,#42385,#42386,#42387,#42388,
#42389,#42390,#42391,#42392,#42393,#42394,#42395,#42396,#42397,#42398,#42399,
#42400,#42401,#42402,#42403,#42404,#42405,#42406,#42407,#42408,#42409,#42410,
#42411,#42412,#42413,#42414,#42415,#42416,#42417,#42418,#42419,#42420,#42421,
#42422,#42423,#42424,#42425,#42426),.UNSPECIFIED.,.F.,.F.,(4,3,3,3,3,3,
3,3,3,3,3,3,3,3,4),(120.495402845628,120.650981398842,121.147487495134,
121.643993591425,122.140499687717,122.637005784008,123.1335118803,123.630017976591,
124.126524072883,124.623030169174,125.119536265466,125.616042361757,126.112548458049,
126.60905455434,126.778588152808),.UNSPECIFIED.);
#343=B_SPLINE_CURVE_WITH_KNOTS('',3,(#42432,#42433,#42434,#42435,#42436,
#42437,#42438,#42439,#42440,#42441,#42442),.UNSPECIFIED.,.F.,.F.,(4,1,1,
1,1,1,1,1,4),(135.088484104361,135.244748524516,135.741254620807,136.237760717099,
136.73426681339,137.230772909682,137.727279005973,138.223785102265,138.639793508071),
 .UNSPECIFIED.);
#344=B_SPLINE_CURVE_WITH_KNOTS('',3,(#42445,#42446,#42447,#42448,#42449,
#42450,#42451,#42452),.UNSPECIFIED.,.F.,.F.,(4,1,1,1,1,4),(135.088484104361,
135.415456602185,135.911962698477,136.408468794768,136.90497489106,137.401480987351),
 .UNSPECIFIED.);
#345=B_SPLINE_CURVE_WITH_KNOTS('',3,(#42457,#42458,#42459,#42460,#42461,
#42462,#42463,#42464,#42465,#42466,#42467,#42468,#42469,#42470,#42471,#42472),
 .UNSPECIFIED.,.F.,.F.,(4,1,1,1,1,1,1,1,1,1,1,1,1,4),(128.805298797182,
129.286675369017,129.783181465309,130.2796875616,130.776193657892,131.272699754183,
131.769205850475,132.265711946766,132.762218043058,133.258724139349,133.755230235641,
134.251736331932,134.748242428224,135.088484104361),.UNSPECIFIED.);
#346=B_SPLINE_CURVE_WITH_KNOTS('',3,(#42473,#42474,#42475,#42476,#42477,
#42478,#42479,#42480,#42481,#42482,#42483,#42484,#42485,#42486,#42487,#42488,
#42489),.UNSPECIFIED.,.F.,.F.,(4,1,1,1,1,1,1,1,1,1,1,1,1,1,4),(128.805298797182,
128.960877350395,129.457383446687,129.953889542979,130.45039563927,130.946901735562,
131.443407831853,131.939913928145,132.436420024436,132.932926120728,133.429432217019,
133.925938313311,134.422444409602,134.918950505894,135.088484104361),
 .UNSPECIFIED.);
#347=B_SPLINE_CURVE_WITH_KNOTS('',3,(#42494,#42495,#42496,#42497,#42498,
#42499,#42500,#42501,#42502,#42503,#42504,#42505,#42506,#42507,#42508,#42509,
#42510),.UNSPECIFIED.,.F.,.F.,(4,1,1,1,1,1,1,1,1,1,1,1,1,1,4),(122.522113490002,
122.832096117227,123.328602213519,123.82510830981,124.321614406102,124.818120502393,
125.314626598685,125.811132694976,126.307638791268,126.804144887559,127.300650983851,
127.797157080143,128.293663176434,128.790169272726,128.805298797182),
 .UNSPECIFIED.);
#348=B_SPLINE_CURVE_WITH_KNOTS('',3,(#42511,#42512,#42513,#42514,#42515,
#42516,#42517,#42518,#42519,#42520,#42521,#42522,#42523,#42524,#42525,#42526),
 .UNSPECIFIED.,.F.,.F.,(4,1,1,1,1,1,1,1,1,1,1,1,1,4),(122.522113490002,
123.002804194897,123.499310291189,123.99581638748,124.492322483772,124.988828580063,
125.485334676355,125.981840772646,126.478346868938,126.974852965229,127.471359061521,
127.967865157812,128.464371254104,128.805298797182),.UNSPECIFIED.);
#349=B_SPLINE_CURVE_WITH_KNOTS('',3,(#42531,#42532,#42533,#42534,#42535,
#42536,#42537,#42538,#42539,#42540,#42541,#42542,#42543,#42544,#42545,#42546,
#42547),.UNSPECIFIED.,.F.,.F.,(4,1,1,1,1,1,1,1,1,1,1,1,1,1,4),(116.238928182822,
116.377516865437,116.874022961729,117.37052905802,117.867035154312,118.363541250603,
118.860047346895,119.356553443186,119.853059539478,120.34956563577,120.846071732061,
121.342577828353,121.839083924644,122.335590020936,122.522113490002),
 .UNSPECIFIED.);
#350=B_SPLINE_CURVE_WITH_KNOTS('',3,(#42548,#42549,#42550,#42551,#42552,
#42553,#42554,#42555,#42556,#42557,#42558,#42559,#42560,#42561,#42562,#42563,
#42564),.UNSPECIFIED.,.F.,.F.,(4,1,1,1,1,1,1,1,1,1,1,1,1,1,4),(116.238928182822,
116.548224943107,117.044731039399,117.54123713569,118.037743231982,118.534249328273,
119.030755424565,119.527261520856,120.023767617148,120.520273713439,121.016779809731,
121.513285906022,122.009792002314,122.506298098606,122.522113490002),
 .UNSPECIFIED.);
#351=B_SPLINE_CURVE_WITH_KNOTS('',3,(#42569,#42570,#42571,#42572,#42573,
#42574,#42575,#42576,#42577,#42578,#42579,#42580,#42581,#42582,#42583,#42584),
 .UNSPECIFIED.,.F.,.F.,(4,1,1,1,1,1,1,1,1,1,1,1,1,4),(109.955742875643,
110.419443709939,110.91594980623,111.412455902522,111.908961998814,112.405468095105,
112.901974191397,113.398480287688,113.89498638398,114.391492480271,114.887998576563,
115.384504672854,115.881010769146,116.238928182822),.UNSPECIFIED.);
#352=B_SPLINE_CURVE_WITH_KNOTS('',3,(#42585,#42586,#42587,#42588,#42589,
#42590,#42591,#42592,#42593,#42594,#42595,#42596,#42597,#42598,#42599,#42600,
#42601),.UNSPECIFIED.,.F.,.F.,(4,1,1,1,1,1,1,1,1,1,1,1,1,1,4),(109.955742875643,
110.093645691317,110.590151787609,111.0866578839,111.583163980192,112.079670076483,
112.576176172775,113.072682269066,113.569188365358,114.06569446165,114.562200557941,
115.058706654233,115.555212750524,116.051718846816,116.238928182822),
 .UNSPECIFIED.);
#353=B_SPLINE_CURVE_WITH_KNOTS('',3,(#42606,#42607,#42608,#42609,#42610,
#42611,#42612,#42613,#42614,#42615,#42616,#42617,#42618,#42619,#42620,#42621,
#42622),.UNSPECIFIED.,.F.,.F.,(4,1,1,1,1,1,1,1,1,1,1,1,1,1,4),(103.672557568463,
103.964864458149,104.461370554441,104.957876650732,105.454382747024,105.950888843315,
106.447394939607,106.943901035898,107.44040713219,107.936913228481,108.433419324773,
108.929925421064,109.426431517356,109.922937613647,109.955742875643),
 .UNSPECIFIED.);
#354=B_SPLINE_CURVE_WITH_KNOTS('',3,(#42623,#42624,#42625,#42626,#42627,
#42628,#42629,#42630,#42631,#42632,#42633,#42634,#42635,#42636,#42637,#42638),
 .UNSPECIFIED.,.F.,.F.,(4,1,1,1,1,1,1,1,1,1,1,1,1,4),(103.672557568463,
104.135572535819,104.63207863211,105.128584728402,105.625090824693,106.121596920985,
106.618103017277,107.114609113568,107.61111520986,108.107621306151,108.604127402443,
109.100633498734,109.597139595026,109.955742875643),.UNSPECIFIED.);
#355=B_SPLINE_CURVE_WITH_KNOTS('',3,(#42643,#42644,#42645,#42646,#42647,
#42648,#42649,#42650,#42651,#42652,#42653,#42654,#42655,#42656,#42657,#42658,
#42659),.UNSPECIFIED.,.F.,.F.,(4,1,1,1,1,1,1,1,1,1,1,1,1,1,4),(97.3893722612836,
97.5102852063591,98.0067913026507,98.5032973989422,98.9998034952337,99.4963095915253,
99.9928156878168,100.489321784108,100.9858278804,101.482333976691,101.978840072983,
102.475346169274,102.971852265566,103.468358361857,103.672557568463),
 .UNSPECIFIED.);
#356=B_SPLINE_CURVE_WITH_KNOTS('',3,(#42660,#42661,#42662,#42663,#42664,
#42665,#42666,#42667,#42668,#42669,#42670,#42671,#42672,#42673,#42674,#42675,
#42676),.UNSPECIFIED.,.F.,.F.,(4,1,1,1,1,1,1,1,1,1,1,1,1,1,4),(97.3893722612836,
97.680993284029,98.1774993803205,98.6740054766121,99.1705115729036,99.6670176691951,
100.163523765487,100.660029861778,101.15653595807,101.653042054361,102.149548150653,
102.646054246944,103.142560343236,103.639066439527,103.672557568463),
 .UNSPECIFIED.);
#357=B_SPLINE_CURVE_WITH_KNOTS('',3,(#42681,#42682,#42683,#42684,#42685,
#42686,#42687,#42688,#42689,#42690,#42691,#42692,#42693,#42694,#42695,#42696),
 .UNSPECIFIED.,.F.,.F.,(4,1,1,1,1,1,1,1,1,1,1,1,1,4),(91.106186954104,91.5522120508608,
92.0487181471523,92.5452242434438,93.0417303397354,93.5382364360269,94.0347425323184,
94.5312486286099,95.0277547249015,95.524260821193,96.0207669174845,96.5172730137761,
97.0137791100676,97.3893722612836),.UNSPECIFIED.);
#358=B_SPLINE_CURVE_WITH_KNOTS('',3,(#42697,#42698,#42699,#42700,#42701,
#42702,#42703,#42704,#42705,#42706,#42707,#42708,#42709,#42710,#42711,#42712,
#42713),.UNSPECIFIED.,.F.,.F.,(4,1,1,1,1,1,1,1,1,1,1,1,1,1,4),(91.106186954104,
91.2264140322391,91.7229201285306,92.2194262248221,92.7159323211137,93.2124384174052,
93.7089445136967,94.2054506099883,94.7019567062798,95.1984628025713,95.6949688988629,
96.1914749951544,96.6879810914459,97.1844871877375,97.3893722612836),
 .UNSPECIFIED.);
#359=B_SPLINE_CURVE_WITH_KNOTS('',3,(#42718,#42719,#42720,#42721,#42722,
#42723,#42724,#42725,#42726,#42727,#42728,#42729,#42730,#42731,#42732,#42733,
#42734),.UNSPECIFIED.,.F.,.F.,(4,1,1,1,1,1,1,1,1,1,1,1,1,1,4),(84.8230016469244,
85.0976327990709,85.5941388953624,86.0906449916539,86.5871510879454,87.083657184237,
87.5801632805285,88.07666937682,88.5731754731116,89.0696815694031,89.5661876656946,
90.0626937619862,90.5591998582777,91.0557059545692,91.106186954104),
 .UNSPECIFIED.);
#360=B_SPLINE_CURVE_WITH_KNOTS('',3,(#42735,#42736,#42737,#42738,#42739,
#42740,#42741,#42742,#42743,#42744,#42745,#42746,#42747,#42748,#42749,#42750),
 .UNSPECIFIED.,.F.,.F.,(4,1,1,1,1,1,1,1,1,1,1,1,1,4),(84.8230016469244,
85.2683408767407,85.7648469730322,86.2613530693238,86.7578591656153,87.2543652619068,
87.7508713581984,88.2473774544899,88.7438835507814,89.240389647073,89.7368957433645,
90.233401839656,90.7299079359476,91.106186954104),.UNSPECIFIED.);
#361=B_SPLINE_CURVE_WITH_KNOTS('',3,(#42755,#42756,#42757,#42758,#42759,
#42760,#42761,#42762,#42763,#42764,#42765,#42766),.UNSPECIFIED.,.F.,.F.,
(4,1,1,1,1,1,1,1,1,4),(78.5398163397448,79.1395596435725,80.1325718361555,
81.1255840287386,82.1185962213217,83.1116084139047,83.6081145101963,84.1046206064878,
84.6011267027793,84.8230016469244),.UNSPECIFIED.);
#362=B_SPLINE_CURVE_WITH_KNOTS('',3,(#42767,#42768,#42769,#42770,#42771,
#42772,#42773,#42774,#42775,#42776,#42777,#42778,#42779,#42780,#42781),
 .UNSPECIFIED.,.F.,.F.,(4,1,1,1,1,1,1,1,1,1,1,1,4),(78.5398163397448,78.8137616249508,
79.8067738175339,80.7997860101169,81.2962921064085,81.7927982027,82.2893042989915,
82.7858103952831,83.2823164915746,83.7788225878661,84.2753286841576,84.7718347804492,
84.8230016469244),.UNSPECIFIED.);
#363=B_SPLINE_CURVE_WITH_KNOTS('',3,(#42786,#42787,#42788,#42789,#42790,
#42791,#42792,#42793,#42794,#42795),.UNSPECIFIED.,.F.,.F.,(4,1,1,1,1,1,
1,4),(72.2566310325652,73.1814864880741,74.1744986806572,75.1675108732402,
76.1605230658233,77.1535352584064,78.1465474509894,78.5398163397448),
 .UNSPECIFIED.);
#364=B_SPLINE_CURVE_WITH_KNOTS('',3,(#42796,#42797,#42798,#42799,#42800,
#42801,#42802,#42803,#42804,#42805),.UNSPECIFIED.,.F.,.F.,(4,1,1,1,1,1,
1,4),(72.2566310325652,72.8556884694524,73.8487006620355,74.8417128546185,
75.8347250472016,76.8277372397847,77.8207494323677,78.5398163397448),
 .UNSPECIFIED.);
#365=B_SPLINE_CURVE_WITH_KNOTS('',3,(#42810,#42811,#42812,#42813,#42814,
#42815,#42816,#42817,#42818,#42819,#42820,#42821,#42822,#42823),
 .UNSPECIFIED.,.F.,.F.,(4,1,1,1,1,1,1,1,1,1,1,4),(65.9734457253856,66.2304011399927,
66.7269072362842,67.2234133325757,67.7199194288673,68.2164255251588,68.7129316214503,
69.2094377177418,70.2024499103249,71.195462102908,72.188474295491,72.2566310325652),
 .UNSPECIFIED.);
#366=B_SPLINE_CURVE_WITH_KNOTS('',3,(#42824,#42825,#42826,#42827,#42828,
#42829,#42830,#42831,#42832,#42833),.UNSPECIFIED.,.F.,.F.,(4,1,1,1,1,1,
1,4),(65.9734457253856,66.897615313954,67.8906275065371,68.8836396991202,
69.8766518917032,70.8696640842863,71.8626762768694,72.2566310325652),
 .UNSPECIFIED.);
#367=B_SPLINE_CURVE_WITH_KNOTS('',3,(#42838,#42839,#42840,#42841,#42842,
#42843,#42844,#42845,#42846,#42847,#42848,#42849,#42850,#42851,#42852,#42853,
#42854),.UNSPECIFIED.,.F.,.F.,(4,1,1,1,1,1,1,1,1,1,1,1,1,1,4),(59.6902604182061,
59.7758218882027,60.2723279844943,60.7688340807858,61.2653401770773,61.7618462733689,
62.2583523696604,62.7548584659519,63.2513645622435,63.747870658535,64.2443767548265,
64.7408828511181,65.2373889474096,65.7338950437011,65.9734457253856),
 .UNSPECIFIED.);
#368=B_SPLINE_CURVE_WITH_KNOTS('',3,(#42855,#42856,#42857,#42858,#42859,
#42860,#42861,#42862,#42863,#42864,#42865,#42866,#42867,#42868,#42869,#42870),
 .UNSPECIFIED.,.F.,.F.,(4,1,1,1,1,1,1,1,1,1,1,1,1,4),(59.690260418206,59.9465299658726,
60.4430360621641,60.9395421584557,61.4360482547472,61.9325543510387,62.4290604473303,
62.9255665436218,63.4220726399133,63.9185787362049,64.4150848324964,64.9115909287879,
65.904603121371,65.9734457253856),.UNSPECIFIED.);
#369=B_SPLINE_CURVE_WITH_KNOTS('',3,(#42875,#42876,#42877,#42878,#42879,
#42880,#42881,#42882,#42883,#42884,#42885,#42886,#42887,#42888,#42889,#42890),
 .UNSPECIFIED.,.F.,.F.,(4,1,1,1,1,1,1,1,1,1,1,1,1,4),(53.4070751110264,
53.8177487327044,54.3142548289959,54.8107609252874,55.307267021579,55.8037731178705,
56.300279214162,56.7967853104536,57.2932914067451,57.7897975030366,58.2863035993281,
58.7828096956197,59.2793157919112,59.6902604182061),.UNSPECIFIED.);
#370=B_SPLINE_CURVE_WITH_KNOTS('',3,(#42891,#42892,#42893,#42894,#42895,
#42896,#42897,#42898,#42899,#42900,#42901,#42902,#42903,#42904,#42905,#42906,
#42907),.UNSPECIFIED.,.F.,.F.,(4,1,1,1,1,1,1,1,1,1,1,1,1,1,4),(53.4070751110264,
53.4919507140827,53.9884568103742,54.4849629066658,54.9814690029573,55.4779750992488,
55.9744811955404,56.4709872918319,56.9674933881234,57.463999484415,57.9605055807065,
58.457011676998,58.9535177732896,59.4500238695811,59.690260418206),
 .UNSPECIFIED.);
#371=B_SPLINE_CURVE_WITH_KNOTS('',3,(#42912,#42913,#42914,#42915,#42916,
#42917,#42918,#42919,#42920,#42921,#42922,#42923,#42924,#42925,#42926,#42927,
#42928),.UNSPECIFIED.,.F.,.F.,(4,1,1,1,1,1,1,1,1,1,1,1,1,1,4),(47.1238898038469,
47.3631694809145,47.859675577206,48.3561816734975,48.8526877697891,49.3491938660806,
49.8456999623721,50.3422060586636,50.8387121549552,51.3352182512467,51.8317243475382,
52.3282304438298,52.8247365401213,53.3212426364128,53.4070751110264),
 .UNSPECIFIED.);
#372=B_SPLINE_CURVE_WITH_KNOTS('',3,(#42929,#42930,#42931,#42932,#42933,
#42934,#42935,#42936,#42937,#42938,#42939,#42940,#42941,#42942,#42943,#42944),
 .UNSPECIFIED.,.F.,.F.,(4,1,1,1,1,1,1,1,1,1,1,1,1,4),(47.1238898038468,
47.5338775585843,48.0303836548759,48.5268897511674,49.0233958474589,49.5199019437505,
50.016408040042,50.5129141363335,51.0094202326251,51.5059263289166,52.0024324252081,
52.4989385214996,52.9954446177912,53.4070751110264),.UNSPECIFIED.);
#373=B_SPLINE_CURVE_WITH_KNOTS('',3,(#42949,#42950,#42951,#42952,#42953,
#42954,#42955,#42956,#42957,#42958,#42959,#42960,#42961,#42962,#42963,#42964,
#42965),.UNSPECIFIED.,.F.,.F.,(4,1,1,1,1,1,1,1,1,1,1,1,1,1,4),(40.8407044966673,
40.9085902291246,41.4050963254161,41.9016024217076,42.3981085179991,42.8946146142907,
43.3911207105822,43.8876268068737,44.3841329031653,44.8806389994568,45.3771450957483,
45.8736511920399,46.3701572883314,46.8666633846229,47.1238898038469),
 .UNSPECIFIED.);
#374=B_SPLINE_CURVE_WITH_KNOTS('',3,(#42966,#42967,#42968,#42969,#42970,
#42971,#42972,#42973,#42974,#42975,#42976,#42977,#42978,#42979,#42980,#42981,
#42982),.UNSPECIFIED.,.F.,.F.,(4,1,1,1,1,1,1,1,1,1,1,1,1,1,4),(40.8407044966672,
41.0792983067944,41.575804403086,42.0723104993775,42.568816595669,43.0653226919606,
43.5618287882521,44.0583348845436,44.5548409808351,45.0513470771267,45.5478531734182,
46.0443592697097,46.5408653660013,47.0373714622928,47.1238898038468),
 .UNSPECIFIED.);
#375=B_SPLINE_CURVE_WITH_KNOTS('',3,(#42987,#42988,#42989,#42990,#42991,
#42992,#42993,#42994,#42995,#42996,#42997,#42998,#42999,#43000,#43001,#43002),
 .UNSPECIFIED.,.F.,.F.,(4,1,1,1,1,1,1,1,1,1,1,1,1,4),(34.5575191894877,
34.9505170736262,35.4470231699177,35.9435292662092,36.4400353625008,36.9365414587923,
37.4330475550838,37.9295536513754,38.4260597476669,38.9225658439584,39.41907194025,
39.9155780365415,40.412084132833,40.8407044966673),.UNSPECIFIED.);
#376=B_SPLINE_CURVE_WITH_KNOTS('',3,(#43003,#43004,#43005,#43006,#43007,
#43008,#43009,#43010,#43011,#43012,#43013,#43014,#43015,#43016,#43017,#43018,
#43019),.UNSPECIFIED.,.F.,.F.,(4,1,1,1,1,1,1,1,1,1,1,1,1,1,4),(34.5575191894876,
34.6247190550045,35.1212251512961,35.6177312475876,36.1142373438791,36.6107434401706,
37.1072495364622,37.6037556327537,38.1002617290452,38.5967678253368,39.0932739216283,
39.5897800179198,40.0862861142114,40.5827922105029,40.8407044966672),
 .UNSPECIFIED.);
#377=B_SPLINE_CURVE_WITH_KNOTS('',3,(#43024,#43025,#43026,#43027,#43028,
#43029,#43030,#43031,#43032,#43033,#43034,#43035,#43036,#43037,#43038,#43039,
#43040),.UNSPECIFIED.,.F.,.F.,(4,1,1,1,1,1,1,1,1,1,1,1,1,1,4),(28.2743338823081,
28.4959378218363,28.9924439181278,29.4889500144193,29.9854561107109,30.4819622070024,
30.9784683032939,31.4749743995855,31.971480495877,32.4679865921685,32.9644926884601,
33.4609987847516,33.9575048810431,34.4540109773346,34.5575191894877),
 .UNSPECIFIED.);
#378=B_SPLINE_CURVE_WITH_KNOTS('',3,(#43041,#43042,#43043,#43044,#43045,
#43046,#43047,#43048,#43049,#43050,#43051,#43052,#43053,#43054,#43055,#43056),
 .UNSPECIFIED.,.F.,.F.,(4,1,1,1,1,1,1,1,1,1,1,1,1,4),(28.274333882308,28.6666458995061,
29.1631519957977,29.6596580920892,30.1561641883807,30.6526702846723,31.1491763809638,
31.6456824772553,32.1421885735469,32.6386946698384,33.1352007661299,33.6317068624215,
34.128212958713,34.5575191894876),.UNSPECIFIED.);
#379=B_SPLINE_CURVE_WITH_KNOTS('',3,(#43061,#43062,#43063,#43064,#43065,
#43066,#43067,#43068,#43069,#43070,#43071,#43072,#43073,#43074,#43075,#43076,
#43077),.UNSPECIFIED.,.F.,.F.,(4,1,1,1,1,1,1,1,1,1,1,1,1,1,4),(21.9911485751285,
22.0413585700464,22.5378646663379,23.0343707626294,23.530876858921,24.0273829552125,
24.523889051504,25.0203951477956,25.5169012440871,26.0134073403786,26.5099134366701,
27.0064195329617,27.5029256292532,27.9994317255447,28.2743338823081),
 .UNSPECIFIED.);
#380=B_SPLINE_CURVE_WITH_KNOTS('',3,(#43078,#43079,#43080,#43081,#43082,
#43083,#43084,#43085,#43086,#43087,#43088,#43089,#43090,#43091,#43092,#43093,
#43094),.UNSPECIFIED.,.F.,.F.,(4,1,1,1,1,1,1,1,1,1,1,1,1,1,4),(21.9911485751285,
22.2120666477162,22.7085727440078,23.2050788402993,23.7015849365908,24.1980910328824,
24.6945971291739,25.1911032254654,25.687609321757,26.1841154180485,26.68062151434,
27.1771276106316,27.6736337069231,28.1701398032146,28.274333882308),
 .UNSPECIFIED.);
#381=B_SPLINE_CURVE_WITH_KNOTS('',3,(#43099,#43100,#43101,#43102,#43103,
#43104,#43105,#43106,#43107,#43108,#43109,#43110,#43111,#43112,#43113,#43114),
 .UNSPECIFIED.,.F.,.F.,(4,1,1,1,1,1,1,1,1,1,1,1,1,4),(15.7079632679489,
16.083285414548,16.5797915108395,17.0762976071311,17.5728037034226,18.0693097997141,
18.5658158960056,19.0623219922972,19.5588280885887,20.0553341848802,20.5518402811718,
21.0483463774633,21.5448524737548,21.9911485751285),.UNSPECIFIED.);
#382=B_SPLINE_CURVE_WITH_KNOTS('',3,(#43115,#43116,#43117,#43118,#43119,
#43120,#43121,#43122,#43123,#43124,#43125,#43126,#43127,#43128,#43129,#43130,
#43131),.UNSPECIFIED.,.F.,.F.,(4,1,1,1,1,1,1,1,1,1,1,1,1,1,4),(15.7079632679489,
15.7574873959263,16.2539934922179,16.7504995885094,17.2470056848009,17.7435117810925,
18.240017877384,18.7365239736755,19.2330300699671,19.7295361662586,20.2260422625501,
20.7225483588416,21.2190544551332,21.7155605514247,21.9911485751285),
 .UNSPECIFIED.);
#383=B_SPLINE_CURVE_WITH_KNOTS('',3,(#43133,#43134,#43135,#43136,#43137,
#43138,#43139,#43140,#43141,#43142,#43143,#43144,#43145,#43146,#43147,#43148,
#43149,#43150,#43151,#43152,#43153,#43154,#43155,#43156,#43157,#43158,#43159,
#43160,#43161,#43162,#43163,#43164,#43165,#43166,#43167,#43168,#43169,#43170,
#43171,#43172,#43173,#43174,#43175,#43176,#43177,#43178,#43179,#43180,#43181,
#43182,#43183,#43184,#43185,#43186,#43187,#43188,#43189,#43190,#43191,#43192,
#43193,#43194,#43195,#43196,#43197,#43198,#43199,#43200,#43201,#43202,#43203,
#43204,#43205,#43206,#43207,#43208,#43209,#43210,#43211,#43212,#43213,#43214,
#43215,#43216,#43217,#43218,#43219,#43220,#43221,#43222,#43223,#43224,#43225,
#43226,#43227,#43228,#43229,#43230,#43231,#43232,#43233,#43234,#43235),
 .UNSPECIFIED.,.F.,.F.,(4,3,3,3,3,3,3,3,3,3,3,3,3,3,3,3,3,3,3,3,3,3,3,3,
3,3,3,3,3,3,3,3,3,3,4),(-0.937740963081824,-0.904523217505006,-0.866625128668399,
-0.845007794788879,-0.830203217768472,-0.823788649298019,-0.784867066646426,
-0.745695756246804,-0.730731146380581,-0.722415114958876,-0.713900080041304,
-0.693686457632239,-0.654578468140619,-0.614852605890178,-0.579246347886379,
-0.552541654383529,-0.547074308466247,-0.506129338035449,-0.472427573874981,
-0.431684200951587,-0.390608431412487,-0.376471022267793,-0.370730708360049,
-0.329054764822938,-0.285097860757189,-0.24114095669144,-0.21099833710501,
-0.197810941035947,-0.189566456838293,-0.18424425154934,-0.141986144540954,
-0.0988362730036117,-0.0555327093168028,-0.0126020697380223,0.),
 .UNSPECIFIED.);
#384=B_SPLINE_CURVE_WITH_KNOTS('',3,(#43238,#43239,#43240,#43241,#43242,
#43243,#43244,#43245,#43246,#43247,#43248,#43249,#43250,#43251,#43252,#43253,
#43254,#43255,#43256,#43257,#43258,#43259,#43260,#43261,#43262,#43263,#43264,
#43265,#43266,#43267,#43268,#43269,#43270,#43271,#43272,#43273,#43274,#43275,
#43276,#43277,#43278,#43279,#43280,#43281,#43282,#43283,#43284,#43285,#43286,
#43287,#43288,#43289,#43290,#43291,#43292,#43293,#43294,#43295,#43296,#43297,
#43298,#43299,#43300,#43301,#43302,#43303,#43304,#43305,#43306,#43307,#43308,
#43309,#43310,#43311,#43312,#43313,#43314,#43315,#43316,#43317,#43318,#43319,
#43320,#43321,#43322,#43323,#43324,#43325,#43326,#43327,#43328,#43329,#43330,
#43331,#43332,#43333,#43334,#43335,#43336,#43337,#43338,#43339,#43340),
 .UNSPECIFIED.,.F.,.F.,(4,3,3,3,3,3,3,3,3,3,3,3,3,3,3,3,3,3,3,3,3,3,3,3,
3,3,3,3,3,3,3,3,3,3,4),(-0.93397589402309,-0.894422503905188,-0.851092289922783,
-0.826729421212481,-0.807865956409088,-0.801823722421914,-0.759290601264971,
-0.717093733962539,-0.686641537101452,-0.680702739992375,-0.656189340240365,
-0.614616501183358,-0.572941838791487,-0.536581284129042,-0.509310868132208,
-0.503319094267446,-0.498509563752087,-0.458073882399315,-0.427499620141708,
-0.386898349768095,-0.346636041099517,-0.332619841408937,-0.324859429439165,
-0.285375022877491,-0.246326502361671,-0.208719056729236,-0.182629174638081,
-0.169421423696199,-0.162163161061763,-0.157293280629028,-0.117969960471771,
-0.079679826239659,-0.0398399131198295,-0.00282314033426902,0.),
 .UNSPECIFIED.);
#385=B_SPLINE_CURVE_WITH_KNOTS('',3,(#44329,#44330,#44331,#44332),
 .UNSPECIFIED.,.F.,.F.,(4,4),(126.778588152808,127.025062960147),
 .UNSPECIFIED.);
#386=B_SPLINE_CURVE_WITH_KNOTS('',3,(#44334,#44335,#44336,#44337,#44338,
#44339,#44340,#44341,#44342,#44343,#44344,#44345,#44346,#44347,#44348,#44349,
#44350,#44351,#44352,#44353,#44354,#44355,#44356,#44357,#44358,#44359,#44360,
#44361,#44362,#44363,#44364,#44365,#44366,#44367,#44368,#44369,#44370,#44371,
#44372,#44373,#44374,#44375,#44376,#44377,#44378,#44379,#44380,#44381,#44382,
#44383,#44384,#44385,#44386,#44387,#44388,#44389,#44390,#44391,#44392,#44393,
#44394,#44395,#44396,#44397,#44398,#44399,#44400,#44401,#44402,#44403,#44404,
#44405,#44406,#44407,#44408,#44409,#44410,#44411,#44412,#44413,#44414,#44415,
#44416,#44417,#44418,#44419,#44420,#44421,#44422,#44423,#44424,#44425,#44426,
#44427,#44428,#44429,#44430,#44431,#44432,#44433,#44434,#44435,#44436),
 .UNSPECIFIED.,.F.,.F.,(4,3,3,3,3,3,3,3,3,3,3,3,3,3,3,3,3,3,3,3,3,3,3,3,
3,3,3,3,3,3,3,3,3,3,4),(-0.937740963081816,-0.904523217504992,-0.866625127455818,
-0.845007793727865,-0.830203217197392,-0.823788648517869,-0.784867065183403,
-0.745695754812804,-0.73073114487324,-0.722415112751658,-0.713900080444087,
-0.693686457632193,-0.654578469885656,-0.614852608246762,-0.579246349653809,
-0.552541655709094,-0.547074309750651,-0.506129339576615,-0.472427573874949,
-0.431684202389108,-0.390608433430914,-0.376471029494825,-0.370730712409322,
-0.329054770401609,-0.285097863546512,-0.241140956691414,-0.210998337104987,
-0.197810941035925,-0.189566457200723,-0.18424425222828,-0.141986138823205,
-0.0988362638567851,-0.0555327002774816,-0.0126020669544512,0.),
 .UNSPECIFIED.);
#387=B_SPLINE_CURVE_WITH_KNOTS('',3,(#44437,#44438,#44439,#44440,#44441,
#44442,#44443,#44444,#44445,#44446,#44447,#44448,#44449,#44450),
 .UNSPECIFIED.,.F.,.F.,(4,1,1,1,1,1,1,1,1,1,1,4),(10.3764180272042,10.792426433011,
11.2889325293026,11.7854386255941,12.2819447218856,12.7784508181771,13.2749569144687,
13.7714630107602,14.2679691070517,14.7644752033433,15.2609812996348,15.7079632679489),
 .UNSPECIFIED.);
#388=B_SPLINE_CURVE_WITH_KNOTS('',3,(#44456,#44457,#44458,#44459,#44460,
#44461,#44462,#44463,#44464,#44465,#44466,#44467,#44468,#44469,#44470,#44471,
#44472,#44473,#44474,#44475,#44476,#44477,#44478,#44479,#44480,#44481,#44482,
#44483,#44484,#44485,#44486,#44487,#44488,#44489,#44490,#44491,#44492,#44493,
#44494,#44495,#44496,#44497,#44498,#44499,#44500,#44501,#44502,#44503,#44504,
#44505,#44506,#44507,#44508,#44509,#44510,#44511,#44512,#44513,#44514,#44515,
#44516,#44517,#44518,#44519,#44520,#44521,#44522,#44523,#44524,#44525,#44526,
#44527,#44528,#44529,#44530,#44531,#44532,#44533,#44534,#44535,#44536,#44537,
#44538,#44539,#44540,#44541,#44542,#44543,#44544,#44545,#44546,#44547,#44548,
#44549,#44550,#44551,#44552,#44553,#44554,#44555,#44556,#44557,#44558),
 .UNSPECIFIED.,.F.,.F.,(4,3,3,3,3,3,3,3,3,3,3,3,3,3,3,3,3,3,3,3,3,3,3,3,
3,3,3,3,3,3,3,3,3,3,4),(-0.933975894023135,-0.894422503905226,-0.851092289888165,
-0.826729421182192,-0.807865956515983,-0.801823722677367,-0.759290601541375,
-0.717093734614832,-0.686641537427605,-0.68070274056291,-0.656189340240378,
-0.614616501299998,-0.572941837912828,-0.536581283470049,-0.509310867637965,
-0.503319090789543,-0.498509560266509,-0.458073876993764,-0.427499620141712,
-0.386898351256557,-0.346636047946469,-0.332619869734945,-0.324859425120058,
-0.28537502006118,-0.246326506168717,-0.208719056729237,-0.182629174638083,
-0.169421424350286,-0.162163163629911,-0.15729328458594,-0.117969963439455,
-0.079679824896869,-0.0398399124484345,-0.00282312955145499,0.),
 .UNSPECIFIED.);
#389=B_SPLINE_CURVE_WITH_KNOTS('',3,(#44561,#44562,#44563,#44564,#44565,
#44566,#44567,#44568,#44569,#44570,#44571,#44572),.UNSPECIFIED.,.F.,.F.,
(4,1,1,1,1,1,1,1,1,4),(11.6147305479242,12.1112366442157,12.6077427405073,
13.1042488367988,13.6007549330903,14.0972610293819,14.5937671256734,15.0902732219649,
15.5867793182565,15.7079632679489),.UNSPECIFIED.);
#390=B_SPLINE_SURFACE_WITH_KNOTS('',3,3,((#33512,#33513,#33514,#33515,#33516,
#33517),(#33518,#33519,#33520,#33521,#33522,#33523),(#33524,#33525,#33526,
#33527,#33528,#33529),(#33530,#33531,#33532,#33533,#33534,#33535)),
 .UNSPECIFIED.,.F.,.F.,.F.,(4,4),(4,1,1,4),(0.,1.),(0.,0.571428571428571,
0.857142857142857,1.),.UNSPECIFIED.);
#391=B_SPLINE_SURFACE_WITH_KNOTS('',3,3,((#33655,#33656,#33657,#33658,#33659,
#33660),(#33661,#33662,#33663,#33664,#33665,#33666),(#33667,#33668,#33669,
#33670,#33671,#33672),(#33673,#33674,#33675,#33676,#33677,#33678)),
 .UNSPECIFIED.,.F.,.F.,.F.,(4,4),(4,1,1,4),(0.,1.),(-1.75610615531805,-1.00348923161032,
-0.501744615805158,5.55111512312578E-16),.UNSPECIFIED.);
#392=B_SPLINE_SURFACE_WITH_KNOTS('',3,3,((#33870,#33871,#33872,#33873,#33874,
#33875),(#33876,#33877,#33878,#33879,#33880,#33881),(#33882,#33883,#33884,
#33885,#33886,#33887),(#33888,#33889,#33890,#33891,#33892,#33893)),
 .UNSPECIFIED.,.F.,.F.,.F.,(4,4),(4,1,1,4),(0.,1.),(0.,0.571428571428571,
0.857142857142857,1.),.UNSPECIFIED.);
#393=B_SPLINE_SURFACE_WITH_KNOTS('',3,3,((#33954,#33955,#33956,#33957,#33958,
#33959,#33960),(#33961,#33962,#33963,#33964,#33965,#33966,#33967),(#33968,
#33969,#33970,#33971,#33972,#33973,#33974),(#33975,#33976,#33977,#33978,
#33979,#33980,#33981)),.UNSPECIFIED.,.F.,.F.,.F.,(4,4),(4,1,1,1,4),(0.,
1.),(-1.75610615531805,-1.25436153951289,-0.752616923707736,-0.501744615805158,
1.11022302462516E-16),.UNSPECIFIED.);
#394=B_SPLINE_SURFACE_WITH_KNOTS('',3,3,((#34225,#34226,#34227,#34228,#34229,
#34230),(#34231,#34232,#34233,#34234,#34235,#34236),(#34237,#34238,#34239,
#34240,#34241,#34242),(#34243,#34244,#34245,#34246,#34247,#34248)),
 .UNSPECIFIED.,.F.,.F.,.F.,(4,4),(4,1,1,4),(0.,1.),(0.,0.571428571428571,
0.857142857142857,1.),.UNSPECIFIED.);
#395=B_SPLINE_SURFACE_WITH_KNOTS('',3,3,((#34365,#34366,#34367,#34368,#34369,
#34370),(#34371,#34372,#34373,#34374,#34375,#34376),(#34377,#34378,#34379,
#34380,#34381,#34382),(#34383,#34384,#34385,#34386,#34387,#34388)),
 .UNSPECIFIED.,.F.,.F.,.F.,(4,4),(4,1,1,4),(0.,1.),(-1.75610615531806,-1.00348923161031,
-0.501744615805142,2.47024622979097E-14),.UNSPECIFIED.);
#396=B_SPLINE_SURFACE_WITH_KNOTS('',3,3,((#34479,#34480,#34481,#34482,#34483,
#34484),(#34485,#34486,#34487,#34488,#34489,#34490),(#34491,#34492,#34493,
#34494,#34495,#34496),(#34497,#34498,#34499,#34500,#34501,#34502)),
 .UNSPECIFIED.,.F.,.F.,.F.,(4,4),(4,1,1,4),(0.,1.),(0.,0.571428571428571,
0.857142857142857,1.),.UNSPECIFIED.);
#397=B_SPLINE_SURFACE_WITH_KNOTS('',3,3,((#34563,#34564,#34565,#34566,#34567,
#34568),(#34569,#34570,#34571,#34572,#34573,#34574),(#34575,#34576,#34577,
#34578,#34579,#34580),(#34581,#34582,#34583,#34584,#34585,#34586)),
 .UNSPECIFIED.,.F.,.F.,.F.,(4,4),(4,1,1,4),(0.,1.),(-1.75610615531805,-1.00348923161031,
-0.501744615805157,-5.27355936696957E-16),.UNSPECIFIED.);
#398=B_SPLINE_SURFACE_WITH_KNOTS('',3,3,((#43341,#43342,#43343,#43344,#43345,
#43346,#43347,#43348,#43349,#43350,#43351,#43352,#43353,#43354,#43355,#43356,
#43357,#43358,#43359,#43360,#43361,#43362,#43363,#43364,#43365,#43366,#43367,
#43368,#43369,#43370,#43371,#43372,#43373,#43374,#43375,#43376,#43377,#43378,
#43379,#43380,#43381,#43382,#43383,#43384,#43385,#43386,#43387,#43388,#43389,
#43390,#43391,#43392,#43393,#43394,#43395,#43396,#43397,#43398,#43399,#43400,
#43401,#43402,#43403,#43404,#43405,#43406,#43407,#43408,#43409,#43410,#43411,
#43412,#43413,#43414,#43415,#43416,#43417,#43418,#43419,#43420,#43421,#43422,
#43423,#43424,#43425,#43426,#43427,#43428,#43429,#43430,#43431,#43432,#43433,
#43434,#43435,#43436,#43437,#43438,#43439,#43440,#43441,#43442,#43443,#43444,
#43445,#43446,#43447,#43448,#43449,#43450,#43451,#43452,#43453,#43454,#43455,
#43456,#43457,#43458,#43459,#43460,#43461,#43462,#43463,#43464,#43465,#43466,
#43467,#43468,#43469,#43470,#43471,#43472,#43473,#43474,#43475,#43476,#43477,
#43478,#43479,#43480,#43481,#43482,#43483,#43484,#43485,#43486,#43487,#43488,
#43489,#43490,#43491,#43492,#43493,#43494,#43495,#43496,#43497,#43498,#43499,
#43500,#43501,#43502,#43503,#43504,#43505,#43506,#43507,#43508,#43509,#43510,
#43511,#43512,#43513,#43514,#43515,#43516,#43517,#43518,#43519,#43520,#43521,
#43522,#43523,#43524,#43525,#43526,#43527,#43528,#43529,#43530,#43531,#43532,
#43533,#43534,#43535,#43536,#43537,#43538,#43539,#43540,#43541,#43542,#43543,
#43544,#43545,#43546,#43547,#43548,#43549,#43550,#43551,#43552,#43553,#43554,
#43555,#43556,#43557,#43558,#43559,#43560,#43561,#43562,#43563,#43564,#43565,
#43566,#43567,#43568,#43569,#43570,#43571,#43572,#43573,#43574,#43575,#43576,
#43577,#43578,#43579,#43580,#43581,#43582,#43583,#43584,#43585,#43586,#43587),
(#43588,#43589,#43590,#43591,#43592,#43593,#43594,#43595,#43596,#43597,
#43598,#43599,#43600,#43601,#43602,#43603,#43604,#43605,#43606,#43607,#43608,
#43609,#43610,#43611,#43612,#43613,#43614,#43615,#43616,#43617,#43618,#43619,
#43620,#43621,#43622,#43623,#43624,#43625,#43626,#43627,#43628,#43629,#43630,
#43631,#43632,#43633,#43634,#43635,#43636,#43637,#43638,#43639,#43640,#43641,
#43642,#43643,#43644,#43645,#43646,#43647,#43648,#43649,#43650,#43651,#43652,
#43653,#43654,#43655,#43656,#43657,#43658,#43659,#43660,#43661,#43662,#43663,
#43664,#43665,#43666,#43667,#43668,#43669,#43670,#43671,#43672,#43673,#43674,
#43675,#43676,#43677,#43678,#43679,#43680,#43681,#43682,#43683,#43684,#43685,
#43686,#43687,#43688,#43689,#43690,#43691,#43692,#43693,#43694,#43695,#43696,
#43697,#43698,#43699,#43700,#43701,#43702,#43703,#43704,#43705,#43706,#43707,
#43708,#43709,#43710,#43711,#43712,#43713,#43714,#43715,#43716,#43717,#43718,
#43719,#43720,#43721,#43722,#43723,#43724,#43725,#43726,#43727,#43728,#43729,
#43730,#43731,#43732,#43733,#43734,#43735,#43736,#43737,#43738,#43739,#43740,
#43741,#43742,#43743,#43744,#43745,#43746,#43747,#43748,#43749,#43750,#43751,
#43752,#43753,#43754,#43755,#43756,#43757,#43758,#43759,#43760,#43761,#43762,
#43763,#43764,#43765,#43766,#43767,#43768,#43769,#43770,#43771,#43772,#43773,
#43774,#43775,#43776,#43777,#43778,#43779,#43780,#43781,#43782,#43783,#43784,
#43785,#43786,#43787,#43788,#43789,#43790,#43791,#43792,#43793,#43794,#43795,
#43796,#43797,#43798,#43799,#43800,#43801,#43802,#43803,#43804,#43805,#43806,
#43807,#43808,#43809,#43810,#43811,#43812,#43813,#43814,#43815,#43816,#43817,
#43818,#43819,#43820,#43821,#43822,#43823,#43824,#43825,#43826,#43827,#43828,
#43829,#43830,#43831,#43832,#43833,#43834),(#43835,#43836,#43837,#43838,
#43839,#43840,#43841,#43842,#43843,#43844,#43845,#43846,#43847,#43848,#43849,
#43850,#43851,#43852,#43853,#43854,#43855,#43856,#43857,#43858,#43859,#43860,
#43861,#43862,#43863,#43864,#43865,#43866,#43867,#43868,#43869,#43870,#43871,
#43872,#43873,#43874,#43875,#43876,#43877,#43878,#43879,#43880,#43881,#43882,
#43883,#43884,#43885,#43886,#43887,#43888,#43889,#43890,#43891,#43892,#43893,
#43894,#43895,#43896,#43897,#43898,#43899,#43900,#43901,#43902,#43903,#43904,
#43905,#43906,#43907,#43908,#43909,#43910,#43911,#43912,#43913,#43914,#43915,
#43916,#43917,#43918,#43919,#43920,#43921,#43922,#43923,#43924,#43925,#43926,
#43927,#43928,#43929,#43930,#43931,#43932,#43933,#43934,#43935,#43936,#43937,
#43938,#43939,#43940,#43941,#43942,#43943,#43944,#43945,#43946,#43947,#43948,
#43949,#43950,#43951,#43952,#43953,#43954,#43955,#43956,#43957,#43958,#43959,
#43960,#43961,#43962,#43963,#43964,#43965,#43966,#43967,#43968,#43969,#43970,
#43971,#43972,#43973,#43974,#43975,#43976,#43977,#43978,#43979,#43980,#43981,
#43982,#43983,#43984,#43985,#43986,#43987,#43988,#43989,#43990,#43991,#43992,
#43993,#43994,#43995,#43996,#43997,#43998,#43999,#44000,#44001,#44002,#44003,
#44004,#44005,#44006,#44007,#44008,#44009,#44010,#44011,#44012,#44013,#44014,
#44015,#44016,#44017,#44018,#44019,#44020,#44021,#44022,#44023,#44024,#44025,
#44026,#44027,#44028,#44029,#44030,#44031,#44032,#44033,#44034,#44035,#44036,
#44037,#44038,#44039,#44040,#44041,#44042,#44043,#44044,#44045,#44046,#44047,
#44048,#44049,#44050,#44051,#44052,#44053,#44054,#44055,#44056,#44057,#44058,
#44059,#44060,#44061,#44062,#44063,#44064,#44065,#44066,#44067,#44068,#44069,
#44070,#44071,#44072,#44073,#44074,#44075,#44076,#44077,#44078,#44079,#44080,
#44081),(#44082,#44083,#44084,#44085,#44086,#44087,#44088,#44089,#44090,
#44091,#44092,#44093,#44094,#44095,#44096,#44097,#44098,#44099,#44100,#44101,
#44102,#44103,#44104,#44105,#44106,#44107,#44108,#44109,#44110,#44111,#44112,
#44113,#44114,#44115,#44116,#44117,#44118,#44119,#44120,#44121,#44122,#44123,
#44124,#44125,#44126,#44127,#44128,#44129,#44130,#44131,#44132,#44133,#44134,
#44135,#44136,#44137,#44138,#44139,#44140,#44141,#44142,#44143,#44144,#44145,
#44146,#44147,#44148,#44149,#44150,#44151,#44152,#44153,#44154,#44155,#44156,
#44157,#44158,#44159,#44160,#44161,#44162,#44163,#44164,#44165,#44166,#44167,
#44168,#44169,#44170,#44171,#44172,#44173,#44174,#44175,#44176,#44177,#44178,
#44179,#44180,#44181,#44182,#44183,#44184,#44185,#44186,#44187,#44188,#44189,
#44190,#44191,#44192,#44193,#44194,#44195,#44196,#44197,#44198,#44199,#44200,
#44201,#44202,#44203,#44204,#44205,#44206,#44207,#44208,#44209,#44210,#44211,
#44212,#44213,#44214,#44215,#44216,#44217,#44218,#44219,#44220,#44221,#44222,
#44223,#44224,#44225,#44226,#44227,#44228,#44229,#44230,#44231,#44232,#44233,
#44234,#44235,#44236,#44237,#44238,#44239,#44240,#44241,#44242,#44243,#44244,
#44245,#44246,#44247,#44248,#44249,#44250,#44251,#44252,#44253,#44254,#44255,
#44256,#44257,#44258,#44259,#44260,#44261,#44262,#44263,#44264,#44265,#44266,
#44267,#44268,#44269,#44270,#44271,#44272,#44273,#44274,#44275,#44276,#44277,
#44278,#44279,#44280,#44281,#44282,#44283,#44284,#44285,#44286,#44287,#44288,
#44289,#44290,#44291,#44292,#44293,#44294,#44295,#44296,#44297,#44298,#44299,
#44300,#44301,#44302,#44303,#44304,#44305,#44306,#44307,#44308,#44309,#44310,
#44311,#44312,#44313,#44314,#44315,#44316,#44317,#44318,#44319,#44320,#44321,
#44322,#44323,#44324,#44325,#44326,#44327,#44328)),.UNSPECIFIED.,.F.,.F.,
 .F.,(4,4),(4,1,1,1,1,1,1,1,1,1,1,1,1,1,1,1,1,1,1,1,1,1,1,1,1,1,1,1,1,1,
1,1,1,1,1,1,1,1,1,1,1,1,1,1,1,1,1,1,1,1,1,1,1,1,1,1,1,1,1,1,1,1,1,1,1,1,
1,1,1,1,1,1,1,1,1,1,1,1,1,1,1,1,1,1,1,1,1,1,1,1,1,1,1,1,1,1,1,1,1,1,1,1,
1,1,1,1,1,1,1,1,1,1,1,1,1,1,1,1,1,1,1,1,1,1,1,1,1,1,1,1,1,1,1,1,1,1,1,1,
1,1,1,1,1,1,1,1,1,1,1,1,1,1,1,1,1,1,1,1,1,1,1,1,1,1,1,1,1,1,1,1,1,1,1,1,
1,1,1,1,1,1,1,1,1,1,1,1,1,1,1,1,1,1,1,1,1,1,1,1,1,1,1,1,1,1,1,1,1,1,1,1,
1,1,1,1,1,1,1,1,1,1,1,1,1,1,1,1,1,1,1,1,1,1,1,1,1,1,1,1,1,1,1,1,1,1,4),
(0.,0.0986691610045074),(8.30989595155336,8.80640204784489,9.30290814413643,
9.79941424042796,10.2959203367195,10.792426433011,11.2889325293026,11.7854386255941,
12.2819447218856,12.7784508181771,13.2749569144687,13.7714630107602,14.2679691070517,
14.7644752033433,15.2609812996348,15.7574873959263,16.2539934922179,16.7504995885094,
17.2470056848009,17.7435117810925,18.240017877384,18.7365239736755,19.2330300699671,
19.7295361662586,20.2260422625501,20.7225483588416,21.2190544551332,21.7155605514247,
22.2120666477162,22.7085727440078,23.2050788402993,23.7015849365908,24.1980910328824,
24.6945971291739,25.1911032254654,25.687609321757,26.1841154180485,26.68062151434,
27.1771276106316,27.6736337069231,28.1701398032146,28.6666458995061,29.1631519957977,
29.6596580920892,30.1561641883807,30.6526702846723,31.1491763809638,31.6456824772553,
32.1421885735469,32.6386946698384,33.1352007661299,33.6317068624215,34.128212958713,
34.6247190550045,35.1212251512961,35.6177312475876,36.1142373438791,36.6107434401706,
37.1072495364622,37.6037556327537,38.1002617290452,38.5967678253368,39.0932739216283,
39.5897800179198,40.0862861142114,40.5827922105029,41.0792983067944,41.575804403086,
42.0723104993775,42.568816595669,43.0653226919606,43.5618287882521,44.0583348845436,
44.5548409808351,45.0513470771267,45.5478531734182,46.0443592697097,46.5408653660013,
47.0373714622928,47.5338775585843,48.0303836548759,48.5268897511674,49.0233958474589,
49.5199019437505,50.016408040042,50.5129141363335,51.0094202326251,51.5059263289166,
52.0024324252081,52.4989385214996,52.9954446177912,53.4919507140827,53.9884568103742,
54.4849629066658,54.9814690029573,55.4779750992488,55.9744811955404,56.4709872918319,
56.9674933881234,57.463999484415,57.9605055807065,58.457011676998,58.9535177732896,
59.4500238695811,59.9465299658726,60.4430360621641,60.9395421584557,61.4360482547472,
61.9325543510387,62.4290604473303,62.9255665436218,63.4220726399133,63.9185787362049,
64.4150848324964,64.9115909287879,65.904603121371,66.897615313954,67.8906275065371,
68.8836396991202,69.8766518917032,70.8696640842863,71.8626762768694,72.8556884694524,
73.8487006620355,74.8417128546185,75.8347250472016,76.8277372397847,77.8207494323677,
78.8137616249508,79.8067738175339,80.7997860101169,81.2962921064085,81.7927982027,
82.2893042989915,82.7858103952831,83.2823164915746,83.7788225878661,84.2753286841576,
84.7718347804492,85.2683408767407,85.7648469730322,86.2613530693238,86.7578591656153,
87.2543652619068,87.7508713581984,88.2473774544899,88.7438835507814,89.240389647073,
89.7368957433645,90.233401839656,90.7299079359476,91.2264140322391,91.7229201285306,
92.2194262248221,92.7159323211137,93.2124384174052,93.7089445136967,94.2054506099883,
94.7019567062798,95.1984628025713,95.6949688988629,96.1914749951544,96.6879810914459,
97.1844871877375,97.680993284029,98.1774993803205,98.6740054766121,99.1705115729036,
99.6670176691951,100.163523765487,100.660029861778,101.15653595807,101.653042054361,
102.149548150653,102.646054246944,103.142560343236,103.639066439527,104.135572535819,
104.63207863211,105.128584728402,105.625090824693,106.121596920985,106.618103017277,
107.114609113568,107.61111520986,108.107621306151,108.604127402443,109.100633498734,
109.597139595026,110.093645691317,110.590151787609,111.0866578839,111.583163980192,
112.079670076483,112.576176172775,113.072682269066,113.569188365358,114.06569446165,
114.562200557941,115.058706654233,115.555212750524,116.051718846816,116.548224943107,
117.044731039399,117.54123713569,118.037743231982,118.534249328273,119.030755424565,
119.527261520856,120.023767617148,120.520273713439,121.016779809731,121.513285906022,
122.009792002314,122.506298098606,123.002804194897,123.499310291189,123.99581638748,
124.492322483772,124.988828580063,125.485334676355,125.981840772646,126.478346868938,
126.974852965229,127.471359061521,127.967865157812,128.464371254104,128.960877350395,
129.457383446687,129.953889542979,130.45039563927,130.946901735562,131.443407831853,
131.939913928145,132.436420024436,132.932926120728,133.429432217019,133.925938313311,
134.422444409602,134.918950505894,135.415456602185,135.911962698477,136.408468794768,
136.90497489106,137.401480987351),.UNSPECIFIED.);
#399=B_SPLINE_SURFACE_WITH_KNOTS('',3,3,((#44573,#44574,#44575,#44576,#44577,
#44578,#44579,#44580,#44581,#44582,#44583,#44584,#44585,#44586,#44587,#44588,
#44589,#44590,#44591,#44592,#44593,#44594,#44595,#44596,#44597,#44598,#44599,
#44600,#44601,#44602,#44603,#44604,#44605,#44606,#44607,#44608,#44609,#44610,
#44611,#44612,#44613,#44614,#44615,#44616,#44617,#44618,#44619,#44620,#44621,
#44622,#44623,#44624,#44625,#44626,#44627,#44628,#44629,#44630,#44631,#44632,
#44633,#44634,#44635,#44636,#44637,#44638,#44639,#44640,#44641,#44642,#44643,
#44644,#44645,#44646,#44647,#44648,#44649,#44650,#44651,#44652,#44653,#44654,
#44655,#44656,#44657,#44658,#44659,#44660,#44661,#44662,#44663,#44664,#44665,
#44666,#44667,#44668,#44669,#44670,#44671,#44672,#44673,#44674,#44675,#44676,
#44677,#44678,#44679,#44680,#44681,#44682,#44683,#44684,#44685,#44686,#44687,
#44688,#44689,#44690,#44691,#44692,#44693,#44694,#44695,#44696,#44697,#44698,
#44699,#44700,#44701,#44702,#44703,#44704,#44705,#44706,#44707,#44708,#44709,
#44710,#44711,#44712,#44713,#44714,#44715,#44716,#44717,#44718,#44719,#44720,
#44721,#44722,#44723,#44724,#44725,#44726,#44727,#44728,#44729,#44730,#44731,
#44732,#44733,#44734,#44735,#44736,#44737,#44738,#44739,#44740,#44741,#44742,
#44743,#44744,#44745,#44746,#44747,#44748,#44749,#44750,#44751,#44752,#44753,
#44754,#44755,#44756,#44757,#44758,#44759,#44760,#44761,#44762,#44763,#44764,
#44765,#44766,#44767,#44768,#44769,#44770,#44771,#44772,#44773,#44774,#44775,
#44776,#44777,#44778,#44779,#44780,#44781,#44782,#44783,#44784,#44785,#44786,
#44787,#44788,#44789,#44790,#44791,#44792,#44793,#44794,#44795,#44796,#44797,
#44798,#44799,#44800,#44801,#44802,#44803,#44804,#44805,#44806,#44807,#44808,
#44809,#44810,#44811,#44812,#44813,#44814,#44815,#44816,#44817,#44818,#44819,
#44820,#44821),(#44822,#44823,#44824,#44825,#44826,#44827,#44828,#44829,
#44830,#44831,#44832,#44833,#44834,#44835,#44836,#44837,#44838,#44839,#44840,
#44841,#44842,#44843,#44844,#44845,#44846,#44847,#44848,#44849,#44850,#44851,
#44852,#44853,#44854,#44855,#44856,#44857,#44858,#44859,#44860,#44861,#44862,
#44863,#44864,#44865,#44866,#44867,#44868,#44869,#44870,#44871,#44872,#44873,
#44874,#44875,#44876,#44877,#44878,#44879,#44880,#44881,#44882,#44883,#44884,
#44885,#44886,#44887,#44888,#44889,#44890,#44891,#44892,#44893,#44894,#44895,
#44896,#44897,#44898,#44899,#44900,#44901,#44902,#44903,#44904,#44905,#44906,
#44907,#44908,#44909,#44910,#44911,#44912,#44913,#44914,#44915,#44916,#44917,
#44918,#44919,#44920,#44921,#44922,#44923,#44924,#44925,#44926,#44927,#44928,
#44929,#44930,#44931,#44932,#44933,#44934,#44935,#44936,#44937,#44938,#44939,
#44940,#44941,#44942,#44943,#44944,#44945,#44946,#44947,#44948,#44949,#44950,
#44951,#44952,#44953,#44954,#44955,#44956,#44957,#44958,#44959,#44960,#44961,
#44962,#44963,#44964,#44965,#44966,#44967,#44968,#44969,#44970,#44971,#44972,
#44973,#44974,#44975,#44976,#44977,#44978,#44979,#44980,#44981,#44982,#44983,
#44984,#44985,#44986,#44987,#44988,#44989,#44990,#44991,#44992,#44993,#44994,
#44995,#44996,#44997,#44998,#44999,#45000,#45001,#45002,#45003,#45004,#45005,
#45006,#45007,#45008,#45009,#45010,#45011,#45012,#45013,#45014,#45015,#45016,
#45017,#45018,#45019,#45020,#45021,#45022,#45023,#45024,#45025,#45026,#45027,
#45028,#45029,#45030,#45031,#45032,#45033,#45034,#45035,#45036,#45037,#45038,
#45039,#45040,#45041,#45042,#45043,#45044,#45045,#45046,#45047,#45048,#45049,
#45050,#45051,#45052,#45053,#45054,#45055,#45056,#45057,#45058,#45059,#45060,
#45061,#45062,#45063,#45064,#45065,#45066,#45067,#45068,#45069,#45070),
(#45071,#45072,#45073,#45074,#45075,#45076,#45077,#45078,#45079,#45080,
#45081,#45082,#45083,#45084,#45085,#45086,#45087,#45088,#45089,#45090,#45091,
#45092,#45093,#45094,#45095,#45096,#45097,#45098,#45099,#45100,#45101,#45102,
#45103,#45104,#45105,#45106,#45107,#45108,#45109,#45110,#45111,#45112,#45113,
#45114,#45115,#45116,#45117,#45118,#45119,#45120,#45121,#45122,#45123,#45124,
#45125,#45126,#45127,#45128,#45129,#45130,#45131,#45132,#45133,#45134,#45135,
#45136,#45137,#45138,#45139,#45140,#45141,#45142,#45143,#45144,#45145,#45146,
#45147,#45148,#45149,#45150,#45151,#45152,#45153,#45154,#45155,#45156,#45157,
#45158,#45159,#45160,#45161,#45162,#45163,#45164,#45165,#45166,#45167,#45168,
#45169,#45170,#45171,#45172,#45173,#45174,#45175,#45176,#45177,#45178,#45179,
#45180,#45181,#45182,#45183,#45184,#45185,#45186,#45187,#45188,#45189,#45190,
#45191,#45192,#45193,#45194,#45195,#45196,#45197,#45198,#45199,#45200,#45201,
#45202,#45203,#45204,#45205,#45206,#45207,#45208,#45209,#45210,#45211,#45212,
#45213,#45214,#45215,#45216,#45217,#45218,#45219,#45220,#45221,#45222,#45223,
#45224,#45225,#45226,#45227,#45228,#45229,#45230,#45231,#45232,#45233,#45234,
#45235,#45236,#45237,#45238,#45239,#45240,#45241,#45242,#45243,#45244,#45245,
#45246,#45247,#45248,#45249,#45250,#45251,#45252,#45253,#45254,#45255,#45256,
#45257,#45258,#45259,#45260,#45261,#45262,#45263,#45264,#45265,#45266,#45267,
#45268,#45269,#45270,#45271,#45272,#45273,#45274,#45275,#45276,#45277,#45278,
#45279,#45280,#45281,#45282,#45283,#45284,#45285,#45286,#45287,#45288,#45289,
#45290,#45291,#45292,#45293,#45294,#45295,#45296,#45297,#45298,#45299,#45300,
#45301,#45302,#45303,#45304,#45305,#45306,#45307,#45308,#45309,#45310,#45311,
#45312,#45313,#45314,#45315,#45316,#45317,#45318,#45319),(#45320,#45321,
#45322,#45323,#45324,#45325,#45326,#45327,#45328,#45329,#45330,#45331,#45332,
#45333,#45334,#45335,#45336,#45337,#45338,#45339,#45340,#45341,#45342,#45343,
#45344,#45345,#45346,#45347,#45348,#45349,#45350,#45351,#45352,#45353,#45354,
#45355,#45356,#45357,#45358,#45359,#45360,#45361,#45362,#45363,#45364,#45365,
#45366,#45367,#45368,#45369,#45370,#45371,#45372,#45373,#45374,#45375,#45376,
#45377,#45378,#45379,#45380,#45381,#45382,#45383,#45384,#45385,#45386,#45387,
#45388,#45389,#45390,#45391,#45392,#45393,#45394,#45395,#45396,#45397,#45398,
#45399,#45400,#45401,#45402,#45403,#45404,#45405,#45406,#45407,#45408,#45409,
#45410,#45411,#45412,#45413,#45414,#45415,#45416,#45417,#45418,#45419,#45420,
#45421,#45422,#45423,#45424,#45425,#45426,#45427,#45428,#45429,#45430,#45431,
#45432,#45433,#45434,#45435,#45436,#45437,#45438,#45439,#45440,#45441,#45442,
#45443,#45444,#45445,#45446,#45447,#45448,#45449,#45450,#45451,#45452,#45453,
#45454,#45455,#45456,#45457,#45458,#45459,#45460,#45461,#45462,#45463,#45464,
#45465,#45466,#45467,#45468,#45469,#45470,#45471,#45472,#45473,#45474,#45475,
#45476,#45477,#45478,#45479,#45480,#45481,#45482,#45483,#45484,#45485,#45486,
#45487,#45488,#45489,#45490,#45491,#45492,#45493,#45494,#45495,#45496,#45497,
#45498,#45499,#45500,#45501,#45502,#45503,#45504,#45505,#45506,#45507,#45508,
#45509,#45510,#45511,#45512,#45513,#45514,#45515,#45516,#45517,#45518,#45519,
#45520,#45521,#45522,#45523,#45524,#45525,#45526,#45527,#45528,#45529,#45530,
#45531,#45532,#45533,#45534,#45535,#45536,#45537,#45538,#45539,#45540,#45541,
#45542,#45543,#45544,#45545,#45546,#45547,#45548,#45549,#45550,#45551,#45552,
#45553,#45554,#45555,#45556,#45557,#45558,#45559,#45560,#45561,#45562,#45563,
#45564,#45565,#45566,#45567,#45568)),.UNSPECIFIED.,.F.,.F.,.F.,(4,4),(4,
1,1,1,1,1,1,1,1,1,1,1,1,1,1,1,1,1,1,1,1,1,1,1,1,1,1,1,1,1,1,1,1,1,1,1,1,
1,1,1,1,1,1,1,1,1,1,1,1,1,1,1,1,1,1,1,1,1,1,1,1,1,1,1,1,1,1,1,1,1,1,1,1,
1,1,1,1,1,1,1,1,1,1,1,1,1,1,1,1,1,1,1,1,1,1,1,1,1,1,1,1,1,1,1,1,1,1,1,1,
1,1,1,1,1,1,1,1,1,1,1,1,1,1,1,1,1,1,1,1,1,1,1,1,1,1,1,1,1,1,1,1,1,1,1,1,
1,1,1,1,1,1,1,1,1,1,1,1,1,1,1,1,1,1,1,1,1,1,1,1,1,1,1,1,1,1,1,1,1,1,1,1,
1,1,1,1,1,1,1,1,1,1,1,1,1,1,1,1,1,1,1,1,1,1,1,1,1,1,1,1,1,1,1,1,1,1,1,1,
1,1,1,1,1,1,1,1,1,1,1,1,1,1,1,1,1,1,1,1,1,1,1,1,1,1,1,1,1,4),(0.,0.0986691610045074),
(11.6147305479242,12.1112366442157,12.6077427405073,13.1042488367988,13.6007549330903,
14.0972610293819,14.5937671256734,15.0902732219649,15.5867793182565,16.083285414548,
16.5797915108395,17.0762976071311,17.5728037034226,18.0693097997141,18.5658158960056,
19.0623219922972,19.5588280885887,20.0553341848802,20.5518402811718,21.0483463774633,
21.5448524737548,22.0413585700464,22.5378646663379,23.0343707626294,23.530876858921,
24.0273829552125,24.523889051504,25.0203951477956,25.5169012440871,26.0134073403786,
26.5099134366701,27.0064195329617,27.5029256292532,27.9994317255447,28.4959378218363,
28.9924439181278,29.4889500144193,29.9854561107109,30.4819622070024,30.9784683032939,
31.4749743995855,31.971480495877,32.4679865921685,32.9644926884601,33.4609987847516,
33.9575048810431,34.4540109773346,34.9505170736262,35.4470231699177,35.9435292662092,
36.4400353625008,36.9365414587923,37.4330475550838,37.9295536513754,38.4260597476669,
38.9225658439584,39.41907194025,39.9155780365415,40.412084132833,40.9085902291246,
41.4050963254161,41.9016024217076,42.3981085179991,42.8946146142907,43.3911207105822,
43.8876268068737,44.3841329031653,44.8806389994568,45.3771450957483,45.8736511920399,
46.3701572883314,46.8666633846229,47.3631694809145,47.859675577206,48.3561816734975,
48.8526877697891,49.3491938660806,49.8456999623721,50.3422060586636,50.8387121549552,
51.3352182512467,51.8317243475382,52.3282304438298,52.8247365401213,53.3212426364128,
53.8177487327044,54.3142548289959,54.8107609252874,55.307267021579,55.8037731178705,
56.300279214162,56.7967853104536,57.2932914067451,57.7897975030366,58.2863035993281,
58.7828096956197,59.2793157919112,59.7758218882027,60.2723279844943,60.7688340807858,
61.2653401770773,61.7618462733689,62.2583523696604,62.7548584659519,63.2513645622435,
63.747870658535,64.2443767548265,64.7408828511181,65.2373889474096,65.7338950437011,
66.2304011399927,66.7269072362842,67.2234133325757,67.7199194288673,68.2164255251588,
68.7129316214503,69.2094377177418,70.2024499103249,71.195462102908,72.188474295491,
73.1814864880741,74.1744986806572,75.1675108732402,76.1605230658233,77.1535352584064,
78.1465474509894,79.1395596435725,80.1325718361555,81.1255840287386,82.1185962213217,
83.1116084139047,83.6081145101963,84.1046206064878,84.6011267027793,85.0976327990709,
85.5941388953624,86.0906449916539,86.5871510879454,87.083657184237,87.5801632805285,
88.07666937682,88.5731754731116,89.0696815694031,89.5661876656946,90.0626937619862,
90.5591998582777,91.0557059545692,91.5522120508608,92.0487181471523,92.5452242434438,
93.0417303397354,93.5382364360269,94.0347425323184,94.5312486286099,95.0277547249015,
95.524260821193,96.0207669174845,96.5172730137761,97.0137791100676,97.5102852063591,
98.0067913026507,98.5032973989422,98.9998034952337,99.4963095915253,99.9928156878168,
100.489321784108,100.9858278804,101.482333976691,101.978840072983,102.475346169274,
102.971852265566,103.468358361857,103.964864458149,104.461370554441,104.957876650732,
105.454382747024,105.950888843315,106.447394939607,106.943901035898,107.44040713219,
107.936913228481,108.433419324773,108.929925421064,109.426431517356,109.922937613647,
110.419443709939,110.91594980623,111.412455902522,111.908961998814,112.405468095105,
112.901974191397,113.398480287688,113.89498638398,114.391492480271,114.887998576563,
115.384504672854,115.881010769146,116.377516865437,116.874022961729,117.37052905802,
117.867035154312,118.363541250603,118.860047346895,119.356553443186,119.853059539478,
120.34956563577,120.846071732061,121.342577828353,121.839083924644,122.335590020936,
122.832096117227,123.328602213519,123.82510830981,124.321614406102,124.818120502393,
125.314626598685,125.811132694976,126.307638791268,126.804144887559,127.300650983851,
127.797157080143,128.293663176434,128.790169272726,129.286675369017,129.783181465309,
130.2796875616,130.776193657892,131.272699754183,131.769205850475,132.265711946766,
132.762218043058,133.258724139349,133.755230235641,134.251736331932,134.748242428224,
135.244748524516,135.741254620807,136.237760717099,136.73426681339,137.230772909682,
137.727279005973,138.223785102265,138.720291198556,139.216797294848,139.713303391139,
140.209809487431,140.706315583722),.UNSPECIFIED.);
#400=CYLINDRICAL_SURFACE('',#25113,9.);
#401=CYLINDRICAL_SURFACE('',#25120,9.);
#402=CYLINDRICAL_SURFACE('',#25126,10.);
#403=CYLINDRICAL_SURFACE('',#25163,1.5);
#404=CYLINDRICAL_SURFACE('',#25166,1.5);
#405=CYLINDRICAL_SURFACE('',#25170,5.05);
#406=CYLINDRICAL_SURFACE('',#25174,5.05);
#407=CYLINDRICAL_SURFACE('',#25177,5.05);
#408=CYLINDRICAL_SURFACE('',#25183,5.05);
#409=CYLINDRICAL_SURFACE('',#25211,5.5);
#410=CYLINDRICAL_SURFACE('',#25215,5.5);
#411=CYLINDRICAL_SURFACE('',#25218,1.5);
#412=CYLINDRICAL_SURFACE('',#25221,1.5);
#413=CYLINDRICAL_SURFACE('',#25238,47.);
#414=CYLINDRICAL_SURFACE('',#25248,1.5);
#415=CYLINDRICAL_SURFACE('',#25249,1.5);
#416=CYLINDRICAL_SURFACE('',#25250,47.);
#417=CYLINDRICAL_SURFACE('',#25253,22.);
#418=CYLINDRICAL_SURFACE('',#25263,1.5);
#419=CYLINDRICAL_SURFACE('',#25264,1.5);
#420=CYLINDRICAL_SURFACE('',#25265,11.);
#421=CYLINDRICAL_SURFACE('',#25268,22.);
#422=CYLINDRICAL_SURFACE('',#25273,47.);
#423=CYLINDRICAL_SURFACE('',#25277,11.);
#424=CYLINDRICAL_SURFACE('',#25279,1.5);
#425=CYLINDRICAL_SURFACE('',#25288,1.5);
#426=CYLINDRICAL_SURFACE('',#25293,1.5);
#427=CYLINDRICAL_SURFACE('',#25295,22.);
#428=CYLINDRICAL_SURFACE('',#25298,22.);
#429=CYLINDRICAL_SURFACE('',#25301,11.);
#430=CYLINDRICAL_SURFACE('',#25303,47.);
#431=CYLINDRICAL_SURFACE('',#25305,1.5);
#432=CYLINDRICAL_SURFACE('',#25311,1.5);
#433=CYLINDRICAL_SURFACE('',#25316,1.5);
#434=CYLINDRICAL_SURFACE('',#25321,1.5);
#435=CYLINDRICAL_SURFACE('',#25325,1.5);
#436=CYLINDRICAL_SURFACE('',#25326,28.);
#437=CYLINDRICAL_SURFACE('',#25329,28.);
#438=CYLINDRICAL_SURFACE('',#25332,28.);
#439=CYLINDRICAL_SURFACE('',#25334,1.5);
#440=CYLINDRICAL_SURFACE('',#25336,1.5);
#441=CYLINDRICAL_SURFACE('',#25340,1.5);
#442=CYLINDRICAL_SURFACE('',#25343,47.);
#443=CYLINDRICAL_SURFACE('',#25346,47.);
#444=CYLINDRICAL_SURFACE('',#25351,1.5);
#445=CYLINDRICAL_SURFACE('',#25355,1.5);
#446=CYLINDRICAL_SURFACE('',#25359,1.5);
#447=CYLINDRICAL_SURFACE('',#25364,1.5);
#448=CYLINDRICAL_SURFACE('',#25369,41.28);
#449=CYLINDRICAL_SURFACE('',#25374,1.5);
#450=CYLINDRICAL_SURFACE('',#25384,1.5);
#451=CYLINDRICAL_SURFACE('',#25390,1.5);
#452=CYLINDRICAL_SURFACE('',#25394,24.55);
#453=CYLINDRICAL_SURFACE('',#25397,1.5);
#454=CYLINDRICAL_SURFACE('',#25403,1.5);
#455=CYLINDRICAL_SURFACE('',#25407,22.45);
#456=CYLINDRICAL_SURFACE('',#25410,22.45);
#457=CYLINDRICAL_SURFACE('',#25413,24.55);
#458=CYLINDRICAL_SURFACE('',#25417,4.01);
#459=CYLINDRICAL_SURFACE('',#25420,4.01);
#460=CYLINDRICAL_SURFACE('',#25426,14.7);
#461=CYLINDRICAL_SURFACE('',#25430,14.3);
#462=CYLINDRICAL_SURFACE('',#25431,14.3);
#463=CYLINDRICAL_SURFACE('',#25433,47.);
#464=CYLINDRICAL_SURFACE('',#25435,11.);
#465=CYLINDRICAL_SURFACE('',#25444,28.);
#466=CYLINDRICAL_SURFACE('',#25449,13.55);
#467=CYLINDRICAL_SURFACE('',#25456,13.55);
#468=CYLINDRICAL_SURFACE('',#25460,0.8);
#469=CYLINDRICAL_SURFACE('',#25467,0.8);
#470=CYLINDRICAL_SURFACE('',#25473,0.8);
#471=CYLINDRICAL_SURFACE('',#25479,0.8);
#472=CYLINDRICAL_SURFACE('',#25484,9.99999999999999);
#473=CYLINDRICAL_SURFACE('',#25487,9.99999999999999);
#474=CYLINDRICAL_SURFACE('',#25500,0.8);
#475=CYLINDRICAL_SURFACE('',#25507,0.8);
#476=CYLINDRICAL_SURFACE('',#25513,0.8);
#477=CYLINDRICAL_SURFACE('',#25518,0.8);
#478=CYLINDRICAL_SURFACE('',#25522,10.);
#479=CYLINDRICAL_SURFACE('',#25524,9.99999999999999);
#480=CYLINDRICAL_SURFACE('',#25534,4.01);
#481=CYLINDRICAL_SURFACE('',#25537,4.01);
#482=CYLINDRICAL_SURFACE('',#25540,4.01);
#483=CYLINDRICAL_SURFACE('',#25543,4.01);
#484=CYLINDRICAL_SURFACE('',#25546,5.3);
#485=CYLINDRICAL_SURFACE('',#25547,5.3);
#486=CYLINDRICAL_SURFACE('',#25548,5.3);
#487=CYLINDRICAL_SURFACE('',#25549,5.3);
#488=CYLINDRICAL_SURFACE('',#25550,8.);
#489=CYLINDRICAL_SURFACE('',#25552,19.3);
#490=CYLINDRICAL_SURFACE('',#25554,21.);
#491=CYLINDRICAL_SURFACE('',#25556,8.);
#492=CYLINDRICAL_SURFACE('',#25558,19.3);
#493=CYLINDRICAL_SURFACE('',#25560,21.);
#494=CYLINDRICAL_SURFACE('',#25568,7.2);
#495=CYLINDRICAL_SURFACE('',#25578,24.55);
#496=CYLINDRICAL_SURFACE('',#25600,22.45);
#497=CYLINDRICAL_SURFACE('',#25608,8.5);
#498=CYLINDRICAL_SURFACE('',#25613,8.5);
#499=CYLINDRICAL_SURFACE('',#25620,8.5);
#500=CYLINDRICAL_SURFACE('',#25626,8.5);
#501=CYLINDRICAL_SURFACE('',#25641,9.99999999999999);
#502=CYLINDRICAL_SURFACE('',#25644,9.99999999999999);
#503=CYLINDRICAL_SURFACE('',#25672,22.45);
#504=CYLINDRICAL_SURFACE('',#25675,24.55);
#505=CYLINDRICAL_SURFACE('',#25679,11.);
#506=CYLINDRICAL_SURFACE('',#25681,4.01);
#507=CYLINDRICAL_SURFACE('',#25684,4.01);
#508=CYLINDRICAL_SURFACE('',#25687,5.3);
#509=CYLINDRICAL_SURFACE('',#25689,5.3);
#510=CYLINDRICAL_SURFACE('',#25691,5.3);
#511=CYLINDRICAL_SURFACE('',#25693,5.3);
#512=CYLINDRICAL_SURFACE('',#25699,9.99999999999999);
#513=CYLINDRICAL_SURFACE('',#25701,10.);
#514=CYLINDRICAL_SURFACE('',#26051,8.5);
#515=CYLINDRICAL_SURFACE('',#26057,7.94);
#516=CYLINDRICAL_SURFACE('',#26060,8.5);
#517=CYLINDRICAL_SURFACE('',#26404,8.5);
#518=CYLINDRICAL_SURFACE('',#26407,8.5);
#519=CYLINDRICAL_SURFACE('',#26421,11.5);
#520=CYLINDRICAL_SURFACE('',#26424,11.5);
#521=CYLINDRICAL_SURFACE('',#26427,19.25);
#522=CYLINDRICAL_SURFACE('',#26430,19.25);
#523=CYLINDRICAL_SURFACE('',#26444,7.94);
#524=CYLINDRICAL_SURFACE('',#26448,14.29);
#525=CYLINDRICAL_SURFACE('',#26452,12.);
#526=CYLINDRICAL_SURFACE('',#26466,12.2);
#527=CYLINDRICAL_SURFACE('',#26479,14.7);
#528=CYLINDRICAL_SURFACE('',#26483,0.800000000000001);
#529=CYLINDRICAL_SURFACE('',#26491,0.800000000000001);
#530=CYLINDRICAL_SURFACE('',#26520,1.);
#531=CYLINDRICAL_SURFACE('',#26527,1.);
#532=CYLINDRICAL_SURFACE('',#26575,7.14);
#533=CYLINDRICAL_SURFACE('',#26579,6.2);
#534=CYLINDRICAL_SURFACE('',#26581,8.5);
#535=CYLINDRICAL_SURFACE('',#26588,10.7);
#536=CYLINDRICAL_SURFACE('',#26590,9.);
#537=CYLINDRICAL_SURFACE('',#26595,11.5);
#538=CYLINDRICAL_SURFACE('',#26599,9.);
#539=CYLINDRICAL_SURFACE('',#26602,10.7);
#540=CYLINDRICAL_SURFACE('',#26606,4.925);
#541=CYLINDRICAL_SURFACE('',#26608,4.925);
#542=CYLINDRICAL_SURFACE('',#26609,4.925);
#543=CYLINDRICAL_SURFACE('',#26610,4.925);
#544=CYLINDRICAL_SURFACE('',#26611,4.925);
#545=CYLINDRICAL_SURFACE('',#26612,4.925);
#546=CYLINDRICAL_SURFACE('',#26613,4.925);
#547=CYLINDRICAL_SURFACE('',#26614,4.925);
#548=CYLINDRICAL_SURFACE('',#26615,4.925);
#549=CYLINDRICAL_SURFACE('',#26616,4.925);
#550=CYLINDRICAL_SURFACE('',#26617,4.925);
#551=CYLINDRICAL_SURFACE('',#26618,4.925);
#552=CYLINDRICAL_SURFACE('',#26619,4.925);
#553=CYLINDRICAL_SURFACE('',#26620,4.925);
#554=CYLINDRICAL_SURFACE('',#26621,4.925);
#555=CYLINDRICAL_SURFACE('',#26622,4.925);
#556=CYLINDRICAL_SURFACE('',#26623,4.925);
#557=CYLINDRICAL_SURFACE('',#26624,4.925);
#558=CYLINDRICAL_SURFACE('',#26625,4.925);
#559=CYLINDRICAL_SURFACE('',#26626,4.925);
#560=CYLINDRICAL_SURFACE('',#26627,4.925);
#561=CYLINDRICAL_SURFACE('',#26629,4.0705);
#562=CYLINDRICAL_SURFACE('',#26631,4.0705);
#563=CYLINDRICAL_SURFACE('',#26632,4.0705);
#564=CYLINDRICAL_SURFACE('',#26633,4.0705);
#565=CYLINDRICAL_SURFACE('',#26634,4.0705);
#566=CYLINDRICAL_SURFACE('',#26635,4.0705);
#567=CYLINDRICAL_SURFACE('',#26636,4.0705);
#568=CYLINDRICAL_SURFACE('',#26637,4.0705);
#569=CYLINDRICAL_SURFACE('',#26638,4.0705);
#570=CYLINDRICAL_SURFACE('',#26639,4.0705);
#571=CYLINDRICAL_SURFACE('',#26640,4.0705);
#572=CYLINDRICAL_SURFACE('',#26641,4.0705);
#573=CYLINDRICAL_SURFACE('',#26642,4.0705);
#574=CYLINDRICAL_SURFACE('',#26643,4.0705);
#575=CYLINDRICAL_SURFACE('',#26644,4.0705);
#576=CYLINDRICAL_SURFACE('',#26645,4.0705);
#577=CYLINDRICAL_SURFACE('',#26646,4.0705);
#578=CYLINDRICAL_SURFACE('',#26647,4.0705);
#579=CYLINDRICAL_SURFACE('',#26648,4.0705);
#580=CYLINDRICAL_SURFACE('',#26649,4.0705);
#581=CYLINDRICAL_SURFACE('',#26656,4.0705);
#582=CYLINDRICAL_SURFACE('',#26885,4.925);
#583=CYLINDRICAL_SURFACE('',#26889,4.95);
#584=CYLINDRICAL_SURFACE('',#26893,8.);
#585=CYLINDRICAL_SURFACE('',#26903,4.);
#586=FACE_BOUND('',#3080,.T.);
#587=FACE_BOUND('',#3084,.T.);
#588=FACE_BOUND('',#3089,.T.);
#589=FACE_BOUND('',#3092,.T.);
#590=FACE_BOUND('',#3097,.T.);
#591=FACE_BOUND('',#3098,.T.);
#592=FACE_BOUND('',#3099,.T.);
#593=FACE_BOUND('',#3100,.T.);
#594=FACE_BOUND('',#3101,.T.);
#595=FACE_BOUND('',#3102,.T.);
#596=FACE_BOUND('',#3122,.T.);
#597=FACE_BOUND('',#3123,.T.);
#598=FACE_BOUND('',#3124,.T.);
#599=FACE_BOUND('',#3125,.T.);
#600=FACE_BOUND('',#3126,.T.);
#601=FACE_BOUND('',#3127,.T.);
#602=FACE_BOUND('',#3128,.T.);
#603=FACE_BOUND('',#3129,.T.);
#604=FACE_BOUND('',#3130,.T.);
#605=FACE_BOUND('',#3228,.T.);
#606=FACE_BOUND('',#3254,.T.);
#607=FACE_BOUND('',#3260,.T.);
#608=FACE_BOUND('',#3263,.T.);
#609=FACE_BOUND('',#3267,.T.);
#610=FACE_BOUND('',#3268,.T.);
#611=FACE_BOUND('',#3282,.T.);
#612=FACE_BOUND('',#3286,.T.);
#613=FACE_BOUND('',#3299,.T.);
#614=FACE_BOUND('',#3301,.T.);
#615=FACE_BOUND('',#3302,.T.);
#616=FACE_BOUND('',#3303,.T.);
#617=FACE_BOUND('',#3304,.T.);
#618=FACE_BOUND('',#3305,.T.);
#619=FACE_BOUND('',#3306,.T.);
#620=FACE_BOUND('',#3307,.T.);
#621=FACE_BOUND('',#3320,.T.);
#622=FACE_BOUND('',#3321,.T.);
#623=FACE_BOUND('',#3322,.T.);
#624=FACE_BOUND('',#3323,.T.);
#625=FACE_BOUND('',#3324,.T.);
#626=FACE_BOUND('',#3325,.T.);
#627=FACE_BOUND('',#3326,.T.);
#628=FACE_BOUND('',#3342,.T.);
#629=FACE_BOUND('',#3347,.T.);
#630=FACE_BOUND('',#3350,.T.);
#631=FACE_BOUND('',#3353,.T.);
#632=FACE_BOUND('',#3362,.T.);
#633=FACE_BOUND('',#3363,.T.);
#634=FACE_BOUND('',#3364,.T.);
#635=FACE_BOUND('',#3365,.T.);
#636=FACE_BOUND('',#3366,.T.);
#637=FACE_BOUND('',#3367,.T.);
#638=FACE_BOUND('',#3368,.T.);
#639=FACE_BOUND('',#3413,.T.);
#640=FACE_BOUND('',#3419,.T.);
#641=FACE_BOUND('',#3431,.T.);
#642=FACE_BOUND('',#3433,.T.);
#643=FACE_BOUND('',#3435,.T.);
#644=FACE_BOUND('',#3437,.T.);
#645=FACE_BOUND('',#3444,.T.);
#646=FACE_BOUND('',#3518,.T.);
#647=FACE_BOUND('',#3791,.T.);
#648=FACE_BOUND('',#3793,.T.);
#649=FACE_BOUND('',#3798,.T.);
#650=FACE_BOUND('',#3872,.T.);
#651=FACE_BOUND('',#4155,.T.);
#652=FACE_BOUND('',#4156,.T.);
#653=FACE_BOUND('',#4157,.T.);
#654=FACE_BOUND('',#4158,.T.);
#655=FACE_BOUND('',#4160,.T.);
#656=FACE_BOUND('',#4161,.T.);
#657=FACE_BOUND('',#4164,.T.);
#658=FACE_BOUND('',#4168,.T.);
#659=FACE_BOUND('',#4171,.T.);
#660=FACE_BOUND('',#4174,.T.);
#661=FACE_BOUND('',#4186,.T.);
#662=FACE_BOUND('',#4187,.T.);
#663=FACE_BOUND('',#4193,.T.);
#664=FACE_BOUND('',#4194,.T.);
#665=FACE_BOUND('',#4242,.T.);
#666=FACE_BOUND('',#4253,.T.);
#667=FACE_BOUND('',#4266,.T.);
#668=FACE_BOUND('',#4270,.T.);
#669=FACE_BOUND('',#4272,.T.);
#670=FACE_BOUND('',#4276,.T.);
#671=FACE_BOUND('',#4279,.T.);
#672=FACE_BOUND('',#4282,.T.);
#673=FACE_BOUND('',#4285,.T.);
#674=FACE_BOUND('',#4489,.T.);
#675=FACE_BOUND('',#4491,.T.);
#676=FACE_BOUND('',#4492,.T.);
#677=FACE_BOUND('',#4493,.T.);
#678=FACE_BOUND('',#4494,.T.);
#679=FACE_BOUND('',#4495,.T.);
#680=FACE_BOUND('',#4496,.T.);
#681=FACE_BOUND('',#4497,.T.);
#682=FACE_BOUND('',#4498,.T.);
#683=FACE_BOUND('',#4499,.T.);
#684=FACE_BOUND('',#4500,.T.);
#685=FACE_BOUND('',#4501,.T.);
#686=FACE_BOUND('',#4502,.T.);
#687=FACE_BOUND('',#4503,.T.);
#688=FACE_BOUND('',#4504,.T.);
#689=FACE_BOUND('',#4505,.T.);
#690=FACE_BOUND('',#4506,.T.);
#691=FACE_BOUND('',#4507,.T.);
#692=FACE_BOUND('',#4508,.T.);
#693=FACE_BOUND('',#4509,.T.);
#694=FACE_BOUND('',#4510,.T.);
#695=FACE_BOUND('',#4511,.T.);
#696=FACE_BOUND('',#4512,.T.);
#697=FACE_BOUND('',#4513,.T.);
#698=FACE_BOUND('',#4514,.T.);
#699=FACE_BOUND('',#4515,.T.);
#700=FACE_BOUND('',#4516,.T.);
#701=FACE_BOUND('',#4517,.T.);
#702=FACE_BOUND('',#4518,.T.);
#703=FACE_BOUND('',#4519,.T.);
#704=FACE_BOUND('',#4520,.T.);
#705=FACE_BOUND('',#4521,.T.);
#706=FACE_BOUND('',#4522,.T.);
#707=FACE_BOUND('',#4523,.T.);
#708=FACE_BOUND('',#4524,.T.);
#709=FACE_BOUND('',#4525,.T.);
#710=FACE_BOUND('',#4528,.T.);
#711=PLANE('',#25111);
#712=PLANE('',#25118);
#713=PLANE('',#25128);
#714=PLANE('',#25132);
#715=PLANE('',#25135);
#716=PLANE('',#25136);
#717=PLANE('',#25164);
#718=PLANE('',#25165);
#719=PLANE('',#25167);
#720=PLANE('',#25176);
#721=PLANE('',#25182);
#722=PLANE('',#25188);
#723=PLANE('',#25189);
#724=PLANE('',#25192);
#725=PLANE('',#25217);
#726=PLANE('',#25219);
#727=PLANE('',#25220);
#728=PLANE('',#25222);
#729=PLANE('',#25225);
#730=PLANE('',#25229);
#731=PLANE('',#25233);
#732=PLANE('',#25234);
#733=PLANE('',#25252);
#734=PLANE('',#25267);
#735=PLANE('',#25294);
#736=PLANE('',#25297);
#737=PLANE('',#25300);
#738=PLANE('',#25328);
#739=PLANE('',#25331);
#740=PLANE('',#25335);
#741=PLANE('',#25337);
#742=PLANE('',#25345);
#743=PLANE('',#25372);
#744=PLANE('',#25375);
#745=PLANE('',#25379);
#746=PLANE('',#25383);
#747=PLANE('',#25396);
#748=PLANE('',#25409);
#749=PLANE('',#25412);
#750=PLANE('',#25415);
#751=PLANE('',#25416);
#752=PLANE('',#25419);
#753=PLANE('',#25422);
#754=PLANE('',#25423);
#755=PLANE('',#25428);
#756=PLANE('',#25432);
#757=PLANE('',#25437);
#758=PLANE('',#25438);
#759=PLANE('',#25439);
#760=PLANE('',#25440);
#761=PLANE('',#25441);
#762=PLANE('',#25442);
#763=PLANE('',#25443);
#764=PLANE('',#25451);
#765=PLANE('',#25458);
#766=PLANE('',#25486);
#767=PLANE('',#25489);
#768=PLANE('',#25491);
#769=PLANE('',#25523);
#770=PLANE('',#25525);
#771=PLANE('',#25536);
#772=PLANE('',#25539);
#773=PLANE('',#25542);
#774=PLANE('',#25545);
#775=PLANE('',#25553);
#776=PLANE('',#25559);
#777=PLANE('',#25561);
#778=PLANE('',#25566);
#779=PLANE('',#25570);
#780=PLANE('',#25574);
#781=PLANE('',#25580);
#782=PLANE('',#25581);
#783=PLANE('',#25592);
#784=PLANE('',#25596);
#785=PLANE('',#25602);
#786=PLANE('',#25603);
#787=PLANE('',#25607);
#788=PLANE('',#25619);
#789=PLANE('',#25630);
#790=PLANE('',#25633);
#791=PLANE('',#25636);
#792=PLANE('',#25639);
#793=PLANE('',#25640);
#794=PLANE('',#25643);
#795=PLANE('',#25646);
#796=PLANE('',#25649);
#797=PLANE('',#25652);
#798=PLANE('',#25656);
#799=PLANE('',#25662);
#800=PLANE('',#25667);
#801=PLANE('',#25670);
#802=PLANE('',#25674);
#803=PLANE('',#25677);
#804=PLANE('',#25678);
#805=PLANE('',#25680);
#806=PLANE('',#25683);
#807=PLANE('',#25686);
#808=PLANE('',#25695);
#809=PLANE('',#25696);
#810=PLANE('',#25697);
#811=PLANE('',#25698);
#812=PLANE('',#25700);
#813=PLANE('',#25702);
#814=PLANE('',#25704);
#815=PLANE('',#25705);
#816=PLANE('',#25707);
#817=PLANE('',#25708);
#818=PLANE('',#25709);
#819=PLANE('',#25710);
#820=PLANE('',#25711);
#821=PLANE('',#25712);
#822=PLANE('',#25713);
#823=PLANE('',#25714);
#824=PLANE('',#25715);
#825=PLANE('',#25716);
#826=PLANE('',#25717);
#827=PLANE('',#25718);
#828=PLANE('',#25719);
#829=PLANE('',#25720);
#830=PLANE('',#25721);
#831=PLANE('',#25722);
#832=PLANE('',#25723);
#833=PLANE('',#25724);
#834=PLANE('',#25725);
#835=PLANE('',#25726);
#836=PLANE('',#25727);
#837=PLANE('',#25728);
#838=PLANE('',#25729);
#839=PLANE('',#25730);
#840=PLANE('',#25731);
#841=PLANE('',#25732);
#842=PLANE('',#25733);
#843=PLANE('',#25734);
#844=PLANE('',#25735);
#845=PLANE('',#25736);
#846=PLANE('',#25737);
#847=PLANE('',#25738);
#848=PLANE('',#25739);
#849=PLANE('',#25740);
#850=PLANE('',#25741);
#851=PLANE('',#25742);
#852=PLANE('',#25743);
#853=PLANE('',#25744);
#854=PLANE('',#25745);
#855=PLANE('',#25746);
#856=PLANE('',#25747);
#857=PLANE('',#25748);
#858=PLANE('',#25749);
#859=PLANE('',#25750);
#860=PLANE('',#25751);
#861=PLANE('',#25752);
#862=PLANE('',#25753);
#863=PLANE('',#25754);
#864=PLANE('',#25755);
#865=PLANE('',#25756);
#866=PLANE('',#25757);
#867=PLANE('',#25758);
#868=PLANE('',#25759);
#869=PLANE('',#25760);
#870=PLANE('',#25761);
#871=PLANE('',#25762);
#872=PLANE('',#25763);
#873=PLANE('',#25764);
#874=PLANE('',#25765);
#875=PLANE('',#25766);
#876=PLANE('',#25767);
#877=PLANE('',#25768);
#878=PLANE('',#25769);
#879=PLANE('',#25770);
#880=PLANE('',#25771);
#881=PLANE('',#25772);
#882=PLANE('',#25773);
#883=PLANE('',#25774);
#884=PLANE('',#25775);
#885=PLANE('',#25776);
#886=PLANE('',#25777);
#887=PLANE('',#25778);
#888=PLANE('',#25779);
#889=PLANE('',#25781);
#890=PLANE('',#25782);
#891=PLANE('',#25783);
#892=PLANE('',#25784);
#893=PLANE('',#25785);
#894=PLANE('',#25786);
#895=PLANE('',#25787);
#896=PLANE('',#25788);
#897=PLANE('',#25789);
#898=PLANE('',#25790);
#899=PLANE('',#25791);
#900=PLANE('',#25792);
#901=PLANE('',#25793);
#902=PLANE('',#25794);
#903=PLANE('',#25795);
#904=PLANE('',#25796);
#905=PLANE('',#25797);
#906=PLANE('',#25798);
#907=PLANE('',#25799);
#908=PLANE('',#25800);
#909=PLANE('',#25801);
#910=PLANE('',#25802);
#911=PLANE('',#25803);
#912=PLANE('',#25804);
#913=PLANE('',#25806);
#914=PLANE('',#25807);
#915=PLANE('',#25808);
#916=PLANE('',#25810);
#917=PLANE('',#25811);
#918=PLANE('',#25812);
#919=PLANE('',#25813);
#920=PLANE('',#25814);
#921=PLANE('',#25815);
#922=PLANE('',#25816);
#923=PLANE('',#25817);
#924=PLANE('',#25818);
#925=PLANE('',#25819);
#926=PLANE('',#25820);
#927=PLANE('',#25821);
#928=PLANE('',#25822);
#929=PLANE('',#25823);
#930=PLANE('',#25824);
#931=PLANE('',#25825);
#932=PLANE('',#25826);
#933=PLANE('',#25827);
#934=PLANE('',#25828);
#935=PLANE('',#25829);
#936=PLANE('',#25830);
#937=PLANE('',#25831);
#938=PLANE('',#25832);
#939=PLANE('',#25833);
#940=PLANE('',#25834);
#941=PLANE('',#25835);
#942=PLANE('',#25836);
#943=PLANE('',#25837);
#944=PLANE('',#25838);
#945=PLANE('',#25839);
#946=PLANE('',#25840);
#947=PLANE('',#25841);
#948=PLANE('',#25842);
#949=PLANE('',#25843);
#950=PLANE('',#25844);
#951=PLANE('',#25845);
#952=PLANE('',#25846);
#953=PLANE('',#25847);
#954=PLANE('',#25848);
#955=PLANE('',#25849);
#956=PLANE('',#25850);
#957=PLANE('',#25851);
#958=PLANE('',#25852);
#959=PLANE('',#25853);
#960=PLANE('',#25854);
#961=PLANE('',#25855);
#962=PLANE('',#25856);
#963=PLANE('',#25857);
#964=PLANE('',#25858);
#965=PLANE('',#25859);
#966=PLANE('',#25860);
#967=PLANE('',#25861);
#968=PLANE('',#25862);
#969=PLANE('',#25863);
#970=PLANE('',#25864);
#971=PLANE('',#25865);
#972=PLANE('',#25866);
#973=PLANE('',#25867);
#974=PLANE('',#25868);
#975=PLANE('',#25869);
#976=PLANE('',#25870);
#977=PLANE('',#25871);
#978=PLANE('',#25872);
#979=PLANE('',#25873);
#980=PLANE('',#25874);
#981=PLANE('',#25875);
#982=PLANE('',#25876);
#983=PLANE('',#25877);
#984=PLANE('',#25878);
#985=PLANE('',#25879);
#986=PLANE('',#25880);
#987=PLANE('',#25881);
#988=PLANE('',#25882);
#989=PLANE('',#25883);
#990=PLANE('',#25884);
#991=PLANE('',#25885);
#992=PLANE('',#25886);
#993=PLANE('',#25887);
#994=PLANE('',#25888);
#995=PLANE('',#25889);
#996=PLANE('',#25890);
#997=PLANE('',#25891);
#998=PLANE('',#25892);
#999=PLANE('',#25893);
#1000=PLANE('',#25894);
#1001=PLANE('',#25895);
#1002=PLANE('',#25896);
#1003=PLANE('',#25897);
#1004=PLANE('',#25898);
#1005=PLANE('',#25899);
#1006=PLANE('',#25900);
#1007=PLANE('',#25901);
#1008=PLANE('',#25902);
#1009=PLANE('',#25903);
#1010=PLANE('',#25904);
#1011=PLANE('',#25905);
#1012=PLANE('',#25906);
#1013=PLANE('',#25907);
#1014=PLANE('',#25908);
#1015=PLANE('',#25909);
#1016=PLANE('',#25910);
#1017=PLANE('',#25911);
#1018=PLANE('',#25912);
#1019=PLANE('',#25913);
#1020=PLANE('',#25914);
#1021=PLANE('',#25915);
#1022=PLANE('',#25916);
#1023=PLANE('',#25917);
#1024=PLANE('',#25918);
#1025=PLANE('',#25919);
#1026=PLANE('',#25920);
#1027=PLANE('',#25921);
#1028=PLANE('',#25922);
#1029=PLANE('',#25923);
#1030=PLANE('',#25924);
#1031=PLANE('',#25925);
#1032=PLANE('',#25926);
#1033=PLANE('',#25927);
#1034=PLANE('',#25928);
#1035=PLANE('',#25929);
#1036=PLANE('',#25930);
#1037=PLANE('',#25931);
#1038=PLANE('',#25932);
#1039=PLANE('',#25933);
#1040=PLANE('',#25934);
#1041=PLANE('',#25935);
#1042=PLANE('',#25936);
#1043=PLANE('',#25937);
#1044=PLANE('',#25938);
#1045=PLANE('',#25939);
#1046=PLANE('',#25940);
#1047=PLANE('',#25941);
#1048=PLANE('',#25942);
#1049=PLANE('',#25943);
#1050=PLANE('',#25944);
#1051=PLANE('',#25945);
#1052=PLANE('',#25946);
#1053=PLANE('',#25947);
#1054=PLANE('',#25948);
#1055=PLANE('',#25949);
#1056=PLANE('',#25950);
#1057=PLANE('',#25951);
#1058=PLANE('',#25952);
#1059=PLANE('',#25953);
#1060=PLANE('',#25954);
#1061=PLANE('',#25955);
#1062=PLANE('',#25956);
#1063=PLANE('',#25957);
#1064=PLANE('',#25958);
#1065=PLANE('',#25959);
#1066=PLANE('',#25960);
#1067=PLANE('',#25961);
#1068=PLANE('',#25962);
#1069=PLANE('',#25963);
#1070=PLANE('',#25964);
#1071=PLANE('',#25965);
#1072=PLANE('',#25966);
#1073=PLANE('',#25967);
#1074=PLANE('',#25968);
#1075=PLANE('',#25969);
#1076=PLANE('',#25970);
#1077=PLANE('',#25971);
#1078=PLANE('',#25972);
#1079=PLANE('',#25973);
#1080=PLANE('',#25974);
#1081=PLANE('',#25975);
#1082=PLANE('',#25976);
#1083=PLANE('',#25977);
#1084=PLANE('',#25978);
#1085=PLANE('',#25979);
#1086=PLANE('',#25980);
#1087=PLANE('',#25981);
#1088=PLANE('',#25982);
#1089=PLANE('',#25983);
#1090=PLANE('',#25984);
#1091=PLANE('',#25985);
#1092=PLANE('',#25986);
#1093=PLANE('',#25987);
#1094=PLANE('',#25988);
#1095=PLANE('',#25989);
#1096=PLANE('',#25990);
#1097=PLANE('',#25991);
#1098=PLANE('',#25992);
#1099=PLANE('',#25993);
#1100=PLANE('',#25994);
#1101=PLANE('',#25995);
#1102=PLANE('',#25996);
#1103=PLANE('',#25997);
#1104=PLANE('',#25998);
#1105=PLANE('',#25999);
#1106=PLANE('',#26000);
#1107=PLANE('',#26001);
#1108=PLANE('',#26002);
#1109=PLANE('',#26003);
#1110=PLANE('',#26004);
#1111=PLANE('',#26005);
#1112=PLANE('',#26006);
#1113=PLANE('',#26007);
#1114=PLANE('',#26008);
#1115=PLANE('',#26009);
#1116=PLANE('',#26010);
#1117=PLANE('',#26011);
#1118=PLANE('',#26012);
#1119=PLANE('',#26013);
#1120=PLANE('',#26014);
#1121=PLANE('',#26015);
#1122=PLANE('',#26016);
#1123=PLANE('',#26017);
#1124=PLANE('',#26018);
#1125=PLANE('',#26019);
#1126=PLANE('',#26020);
#1127=PLANE('',#26021);
#1128=PLANE('',#26022);
#1129=PLANE('',#26023);
#1130=PLANE('',#26024);
#1131=PLANE('',#26025);
#1132=PLANE('',#26026);
#1133=PLANE('',#26027);
#1134=PLANE('',#26028);
#1135=PLANE('',#26029);
#1136=PLANE('',#26030);
#1137=PLANE('',#26031);
#1138=PLANE('',#26032);
#1139=PLANE('',#26033);
#1140=PLANE('',#26034);
#1141=PLANE('',#26035);
#1142=PLANE('',#26036);
#1143=PLANE('',#26037);
#1144=PLANE('',#26038);
#1145=PLANE('',#26039);
#1146=PLANE('',#26040);
#1147=PLANE('',#26041);
#1148=PLANE('',#26042);
#1149=PLANE('',#26043);
#1150=PLANE('',#26044);
#1151=PLANE('',#26045);
#1152=PLANE('',#26046);
#1153=PLANE('',#26047);
#1154=PLANE('',#26048);
#1155=PLANE('',#26049);
#1156=PLANE('',#26050);
#1157=PLANE('',#26053);
#1158=PLANE('',#26059);
#1159=PLANE('',#26062);
#1160=PLANE('',#26064);
#1161=PLANE('',#26065);
#1162=PLANE('',#26067);
#1163=PLANE('',#26068);
#1164=PLANE('',#26069);
#1165=PLANE('',#26070);
#1166=PLANE('',#26071);
#1167=PLANE('',#26072);
#1168=PLANE('',#26073);
#1169=PLANE('',#26074);
#1170=PLANE('',#26075);
#1171=PLANE('',#26076);
#1172=PLANE('',#26077);
#1173=PLANE('',#26078);
#1174=PLANE('',#26079);
#1175=PLANE('',#26080);
#1176=PLANE('',#26081);
#1177=PLANE('',#26082);
#1178=PLANE('',#26083);
#1179=PLANE('',#26084);
#1180=PLANE('',#26085);
#1181=PLANE('',#26086);
#1182=PLANE('',#26087);
#1183=PLANE('',#26088);
#1184=PLANE('',#26089);
#1185=PLANE('',#26090);
#1186=PLANE('',#26091);
#1187=PLANE('',#26092);
#1188=PLANE('',#26093);
#1189=PLANE('',#26094);
#1190=PLANE('',#26095);
#1191=PLANE('',#26096);
#1192=PLANE('',#26097);
#1193=PLANE('',#26098);
#1194=PLANE('',#26099);
#1195=PLANE('',#26100);
#1196=PLANE('',#26101);
#1197=PLANE('',#26102);
#1198=PLANE('',#26103);
#1199=PLANE('',#26104);
#1200=PLANE('',#26105);
#1201=PLANE('',#26106);
#1202=PLANE('',#26107);
#1203=PLANE('',#26108);
#1204=PLANE('',#26109);
#1205=PLANE('',#26110);
#1206=PLANE('',#26111);
#1207=PLANE('',#26112);
#1208=PLANE('',#26113);
#1209=PLANE('',#26114);
#1210=PLANE('',#26115);
#1211=PLANE('',#26116);
#1212=PLANE('',#26117);
#1213=PLANE('',#26118);
#1214=PLANE('',#26119);
#1215=PLANE('',#26120);
#1216=PLANE('',#26121);
#1217=PLANE('',#26122);
#1218=PLANE('',#26123);
#1219=PLANE('',#26124);
#1220=PLANE('',#26125);
#1221=PLANE('',#26126);
#1222=PLANE('',#26127);
#1223=PLANE('',#26128);
#1224=PLANE('',#26129);
#1225=PLANE('',#26130);
#1226=PLANE('',#26131);
#1227=PLANE('',#26132);
#1228=PLANE('',#26133);
#1229=PLANE('',#26134);
#1230=PLANE('',#26135);
#1231=PLANE('',#26136);
#1232=PLANE('',#26137);
#1233=PLANE('',#26138);
#1234=PLANE('',#26139);
#1235=PLANE('',#26141);
#1236=PLANE('',#26142);
#1237=PLANE('',#26143);
#1238=PLANE('',#26144);
#1239=PLANE('',#26145);
#1240=PLANE('',#26146);
#1241=PLANE('',#26147);
#1242=PLANE('',#26148);
#1243=PLANE('',#26149);
#1244=PLANE('',#26150);
#1245=PLANE('',#26151);
#1246=PLANE('',#26152);
#1247=PLANE('',#26153);
#1248=PLANE('',#26154);
#1249=PLANE('',#26155);
#1250=PLANE('',#26156);
#1251=PLANE('',#26157);
#1252=PLANE('',#26158);
#1253=PLANE('',#26159);
#1254=PLANE('',#26160);
#1255=PLANE('',#26161);
#1256=PLANE('',#26162);
#1257=PLANE('',#26163);
#1258=PLANE('',#26164);
#1259=PLANE('',#26165);
#1260=PLANE('',#26166);
#1261=PLANE('',#26167);
#1262=PLANE('',#26168);
#1263=PLANE('',#26169);
#1264=PLANE('',#26170);
#1265=PLANE('',#26171);
#1266=PLANE('',#26172);
#1267=PLANE('',#26173);
#1268=PLANE('',#26174);
#1269=PLANE('',#26175);
#1270=PLANE('',#26176);
#1271=PLANE('',#26177);
#1272=PLANE('',#26178);
#1273=PLANE('',#26179);
#1274=PLANE('',#26180);
#1275=PLANE('',#26181);
#1276=PLANE('',#26182);
#1277=PLANE('',#26183);
#1278=PLANE('',#26184);
#1279=PLANE('',#26185);
#1280=PLANE('',#26186);
#1281=PLANE('',#26187);
#1282=PLANE('',#26188);
#1283=PLANE('',#26189);
#1284=PLANE('',#26190);
#1285=PLANE('',#26191);
#1286=PLANE('',#26192);
#1287=PLANE('',#26193);
#1288=PLANE('',#26194);
#1289=PLANE('',#26195);
#1290=PLANE('',#26196);
#1291=PLANE('',#26197);
#1292=PLANE('',#26198);
#1293=PLANE('',#26199);
#1294=PLANE('',#26200);
#1295=PLANE('',#26201);
#1296=PLANE('',#26202);
#1297=PLANE('',#26203);
#1298=PLANE('',#26204);
#1299=PLANE('',#26205);
#1300=PLANE('',#26206);
#1301=PLANE('',#26207);
#1302=PLANE('',#26208);
#1303=PLANE('',#26209);
#1304=PLANE('',#26210);
#1305=PLANE('',#26211);
#1306=PLANE('',#26212);
#1307=PLANE('',#26213);
#1308=PLANE('',#26214);
#1309=PLANE('',#26215);
#1310=PLANE('',#26216);
#1311=PLANE('',#26217);
#1312=PLANE('',#26218);
#1313=PLANE('',#26219);
#1314=PLANE('',#26220);
#1315=PLANE('',#26221);
#1316=PLANE('',#26222);
#1317=PLANE('',#26223);
#1318=PLANE('',#26224);
#1319=PLANE('',#26225);
#1320=PLANE('',#26226);
#1321=PLANE('',#26227);
#1322=PLANE('',#26228);
#1323=PLANE('',#26229);
#1324=PLANE('',#26230);
#1325=PLANE('',#26231);
#1326=PLANE('',#26232);
#1327=PLANE('',#26233);
#1328=PLANE('',#26234);
#1329=PLANE('',#26235);
#1330=PLANE('',#26236);
#1331=PLANE('',#26237);
#1332=PLANE('',#26238);
#1333=PLANE('',#26239);
#1334=PLANE('',#26240);
#1335=PLANE('',#26241);
#1336=PLANE('',#26242);
#1337=PLANE('',#26243);
#1338=PLANE('',#26244);
#1339=PLANE('',#26245);
#1340=PLANE('',#26246);
#1341=PLANE('',#26247);
#1342=PLANE('',#26248);
#1343=PLANE('',#26249);
#1344=PLANE('',#26250);
#1345=PLANE('',#26251);
#1346=PLANE('',#26252);
#1347=PLANE('',#26253);
#1348=PLANE('',#26254);
#1349=PLANE('',#26255);
#1350=PLANE('',#26256);
#1351=PLANE('',#26257);
#1352=PLANE('',#26258);
#1353=PLANE('',#26259);
#1354=PLANE('',#26260);
#1355=PLANE('',#26261);
#1356=PLANE('',#26262);
#1357=PLANE('',#26263);
#1358=PLANE('',#26264);
#1359=PLANE('',#26265);
#1360=PLANE('',#26266);
#1361=PLANE('',#26267);
#1362=PLANE('',#26268);
#1363=PLANE('',#26269);
#1364=PLANE('',#26270);
#1365=PLANE('',#26271);
#1366=PLANE('',#26272);
#1367=PLANE('',#26273);
#1368=PLANE('',#26274);
#1369=PLANE('',#26275);
#1370=PLANE('',#26276);
#1371=PLANE('',#26277);
#1372=PLANE('',#26278);
#1373=PLANE('',#26279);
#1374=PLANE('',#26280);
#1375=PLANE('',#26281);
#1376=PLANE('',#26282);
#1377=PLANE('',#26283);
#1378=PLANE('',#26284);
#1379=PLANE('',#26285);
#1380=PLANE('',#26286);
#1381=PLANE('',#26287);
#1382=PLANE('',#26288);
#1383=PLANE('',#26289);
#1384=PLANE('',#26290);
#1385=PLANE('',#26291);
#1386=PLANE('',#26292);
#1387=PLANE('',#26293);
#1388=PLANE('',#26294);
#1389=PLANE('',#26295);
#1390=PLANE('',#26296);
#1391=PLANE('',#26297);
#1392=PLANE('',#26298);
#1393=PLANE('',#26299);
#1394=PLANE('',#26300);
#1395=PLANE('',#26301);
#1396=PLANE('',#26302);
#1397=PLANE('',#26303);
#1398=PLANE('',#26304);
#1399=PLANE('',#26305);
#1400=PLANE('',#26306);
#1401=PLANE('',#26307);
#1402=PLANE('',#26308);
#1403=PLANE('',#26309);
#1404=PLANE('',#26310);
#1405=PLANE('',#26311);
#1406=PLANE('',#26312);
#1407=PLANE('',#26313);
#1408=PLANE('',#26314);
#1409=PLANE('',#26315);
#1410=PLANE('',#26316);
#1411=PLANE('',#26317);
#1412=PLANE('',#26318);
#1413=PLANE('',#26319);
#1414=PLANE('',#26320);
#1415=PLANE('',#26321);
#1416=PLANE('',#26322);
#1417=PLANE('',#26323);
#1418=PLANE('',#26324);
#1419=PLANE('',#26325);
#1420=PLANE('',#26326);
#1421=PLANE('',#26327);
#1422=PLANE('',#26328);
#1423=PLANE('',#26329);
#1424=PLANE('',#26330);
#1425=PLANE('',#26331);
#1426=PLANE('',#26332);
#1427=PLANE('',#26333);
#1428=PLANE('',#26334);
#1429=PLANE('',#26335);
#1430=PLANE('',#26336);
#1431=PLANE('',#26337);
#1432=PLANE('',#26338);
#1433=PLANE('',#26339);
#1434=PLANE('',#26340);
#1435=PLANE('',#26341);
#1436=PLANE('',#26342);
#1437=PLANE('',#26343);
#1438=PLANE('',#26344);
#1439=PLANE('',#26345);
#1440=PLANE('',#26346);
#1441=PLANE('',#26347);
#1442=PLANE('',#26348);
#1443=PLANE('',#26349);
#1444=PLANE('',#26350);
#1445=PLANE('',#26351);
#1446=PLANE('',#26352);
#1447=PLANE('',#26353);
#1448=PLANE('',#26354);
#1449=PLANE('',#26355);
#1450=PLANE('',#26356);
#1451=PLANE('',#26357);
#1452=PLANE('',#26358);
#1453=PLANE('',#26359);
#1454=PLANE('',#26360);
#1455=PLANE('',#26361);
#1456=PLANE('',#26362);
#1457=PLANE('',#26363);
#1458=PLANE('',#26364);
#1459=PLANE('',#26365);
#1460=PLANE('',#26366);
#1461=PLANE('',#26367);
#1462=PLANE('',#26368);
#1463=PLANE('',#26369);
#1464=PLANE('',#26370);
#1465=PLANE('',#26371);
#1466=PLANE('',#26372);
#1467=PLANE('',#26373);
#1468=PLANE('',#26374);
#1469=PLANE('',#26375);
#1470=PLANE('',#26376);
#1471=PLANE('',#26377);
#1472=PLANE('',#26378);
#1473=PLANE('',#26379);
#1474=PLANE('',#26380);
#1475=PLANE('',#26381);
#1476=PLANE('',#26382);
#1477=PLANE('',#26383);
#1478=PLANE('',#26384);
#1479=PLANE('',#26385);
#1480=PLANE('',#26386);
#1481=PLANE('',#26387);
#1482=PLANE('',#26388);
#1483=PLANE('',#26389);
#1484=PLANE('',#26390);
#1485=PLANE('',#26391);
#1486=PLANE('',#26392);
#1487=PLANE('',#26393);
#1488=PLANE('',#26394);
#1489=PLANE('',#26395);
#1490=PLANE('',#26396);
#1491=PLANE('',#26397);
#1492=PLANE('',#26398);
#1493=PLANE('',#26399);
#1494=PLANE('',#26400);
#1495=PLANE('',#26401);
#1496=PLANE('',#26402);
#1497=PLANE('',#26403);
#1498=PLANE('',#26406);
#1499=PLANE('',#26409);
#1500=PLANE('',#26411);
#1501=PLANE('',#26412);
#1502=PLANE('',#26413);
#1503=PLANE('',#26414);
#1504=PLANE('',#26415);
#1505=PLANE('',#26416);
#1506=PLANE('',#26417);
#1507=PLANE('',#26418);
#1508=PLANE('',#26419);
#1509=PLANE('',#26420);
#1510=PLANE('',#26433);
#1511=PLANE('',#26434);
#1512=PLANE('',#26440);
#1513=PLANE('',#26446);
#1514=PLANE('',#26450);
#1515=PLANE('',#26454);
#1516=PLANE('',#26458);
#1517=PLANE('',#26463);
#1518=PLANE('',#26465);
#1519=PLANE('',#26468);
#1520=PLANE('',#26469);
#1521=PLANE('',#26473);
#1522=PLANE('',#26475);
#1523=PLANE('',#26487);
#1524=PLANE('',#26495);
#1525=PLANE('',#26496);
#1526=PLANE('',#26497);
#1527=PLANE('',#26498);
#1528=PLANE('',#26499);
#1529=PLANE('',#26500);
#1530=PLANE('',#26501);
#1531=PLANE('',#26502);
#1532=PLANE('',#26503);
#1533=PLANE('',#26504);
#1534=PLANE('',#26505);
#1535=PLANE('',#26506);
#1536=PLANE('',#26507);
#1537=PLANE('',#26508);
#1538=PLANE('',#26509);
#1539=PLANE('',#26510);
#1540=PLANE('',#26511);
#1541=PLANE('',#26512);
#1542=PLANE('',#26529);
#1543=PLANE('',#26530);
#1544=PLANE('',#26531);
#1545=PLANE('',#26532);
#1546=PLANE('',#26533);
#1547=PLANE('',#26534);
#1548=PLANE('',#26535);
#1549=PLANE('',#26536);
#1550=PLANE('',#26537);
#1551=PLANE('',#26538);
#1552=PLANE('',#26539);
#1553=PLANE('',#26540);
#1554=PLANE('',#26541);
#1555=PLANE('',#26542);
#1556=PLANE('',#26543);
#1557=PLANE('',#26544);
#1558=PLANE('',#26545);
#1559=PLANE('',#26546);
#1560=PLANE('',#26547);
#1561=PLANE('',#26548);
#1562=PLANE('',#26549);
#1563=PLANE('',#26550);
#1564=PLANE('',#26552);
#1565=PLANE('',#26553);
#1566=PLANE('',#26554);
#1567=PLANE('',#26555);
#1568=PLANE('',#26556);
#1569=PLANE('',#26557);
#1570=PLANE('',#26558);
#1571=PLANE('',#26559);
#1572=PLANE('',#26560);
#1573=PLANE('',#26561);
#1574=PLANE('',#26563);
#1575=PLANE('',#26564);
#1576=PLANE('',#26565);
#1577=PLANE('',#26566);
#1578=PLANE('',#26568);
#1579=PLANE('',#26569);
#1580=PLANE('',#26570);
#1581=PLANE('',#26571);
#1582=PLANE('',#26577);
#1583=PLANE('',#26584);
#1584=PLANE('',#26586);
#1585=PLANE('',#26593);
#1586=PLANE('',#26597);
#1587=PLANE('',#26601);
#1588=PLANE('',#26604);
#1589=PLANE('',#26650);
#1590=PLANE('',#26652);
#1591=PLANE('',#26657);
#1592=PLANE('',#26658);
#1593=PLANE('',#26660);
#1594=PLANE('',#26661);
#1595=PLANE('',#26663);
#1596=PLANE('',#26664);
#1597=PLANE('',#26666);
#1598=PLANE('',#26667);
#1599=PLANE('',#26669);
#1600=PLANE('',#26670);
#1601=PLANE('',#26672);
#1602=PLANE('',#26673);
#1603=PLANE('',#26675);
#1604=PLANE('',#26676);
#1605=PLANE('',#26678);
#1606=PLANE('',#26679);
#1607=PLANE('',#26681);
#1608=PLANE('',#26682);
#1609=PLANE('',#26684);
#1610=PLANE('',#26685);
#1611=PLANE('',#26687);
#1612=PLANE('',#26688);
#1613=PLANE('',#26690);
#1614=PLANE('',#26691);
#1615=PLANE('',#26693);
#1616=PLANE('',#26694);
#1617=PLANE('',#26696);
#1618=PLANE('',#26697);
#1619=PLANE('',#26699);
#1620=PLANE('',#26700);
#1621=PLANE('',#26702);
#1622=PLANE('',#26703);
#1623=PLANE('',#26705);
#1624=PLANE('',#26706);
#1625=PLANE('',#26708);
#1626=PLANE('',#26709);
#1627=PLANE('',#26711);
#1628=PLANE('',#26712);
#1629=PLANE('',#26714);
#1630=PLANE('',#26715);
#1631=PLANE('',#26717);
#1632=PLANE('',#26718);
#1633=PLANE('',#26720);
#1634=PLANE('',#26721);
#1635=PLANE('',#26723);
#1636=PLANE('',#26724);
#1637=PLANE('',#26726);
#1638=PLANE('',#26727);
#1639=PLANE('',#26729);
#1640=PLANE('',#26730);
#1641=PLANE('',#26732);
#1642=PLANE('',#26733);
#1643=PLANE('',#26735);
#1644=PLANE('',#26736);
#1645=PLANE('',#26738);
#1646=PLANE('',#26739);
#1647=PLANE('',#26741);
#1648=PLANE('',#26742);
#1649=PLANE('',#26744);
#1650=PLANE('',#26745);
#1651=PLANE('',#26747);
#1652=PLANE('',#26748);
#1653=PLANE('',#26750);
#1654=PLANE('',#26751);
#1655=PLANE('',#26753);
#1656=PLANE('',#26754);
#1657=PLANE('',#26756);
#1658=PLANE('',#26757);
#1659=PLANE('',#26759);
#1660=PLANE('',#26760);
#1661=PLANE('',#26763);
#1662=PLANE('',#26764);
#1663=PLANE('',#26767);
#1664=PLANE('',#26768);
#1665=PLANE('',#26770);
#1666=PLANE('',#26771);
#1667=PLANE('',#26773);
#1668=PLANE('',#26774);
#1669=PLANE('',#26776);
#1670=PLANE('',#26777);
#1671=PLANE('',#26779);
#1672=PLANE('',#26780);
#1673=PLANE('',#26782);
#1674=PLANE('',#26783);
#1675=PLANE('',#26785);
#1676=PLANE('',#26786);
#1677=PLANE('',#26788);
#1678=PLANE('',#26789);
#1679=PLANE('',#26791);
#1680=PLANE('',#26792);
#1681=PLANE('',#26794);
#1682=PLANE('',#26795);
#1683=PLANE('',#26797);
#1684=PLANE('',#26798);
#1685=PLANE('',#26800);
#1686=PLANE('',#26801);
#1687=PLANE('',#26803);
#1688=PLANE('',#26804);
#1689=PLANE('',#26806);
#1690=PLANE('',#26807);
#1691=PLANE('',#26809);
#1692=PLANE('',#26810);
#1693=PLANE('',#26812);
#1694=PLANE('',#26813);
#1695=PLANE('',#26815);
#1696=PLANE('',#26816);
#1697=PLANE('',#26818);
#1698=PLANE('',#26819);
#1699=PLANE('',#26821);
#1700=PLANE('',#26822);
#1701=PLANE('',#26824);
#1702=PLANE('',#26825);
#1703=PLANE('',#26827);
#1704=PLANE('',#26828);
#1705=PLANE('',#26830);
#1706=PLANE('',#26831);
#1707=PLANE('',#26833);
#1708=PLANE('',#26834);
#1709=PLANE('',#26836);
#1710=PLANE('',#26837);
#1711=PLANE('',#26839);
#1712=PLANE('',#26840);
#1713=PLANE('',#26842);
#1714=PLANE('',#26843);
#1715=PLANE('',#26845);
#1716=PLANE('',#26846);
#1717=PLANE('',#26848);
#1718=PLANE('',#26849);
#1719=PLANE('',#26851);
#1720=PLANE('',#26852);
#1721=PLANE('',#26854);
#1722=PLANE('',#26855);
#1723=PLANE('',#26857);
#1724=PLANE('',#26858);
#1725=PLANE('',#26860);
#1726=PLANE('',#26861);
#1727=PLANE('',#26863);
#1728=PLANE('',#26864);
#1729=PLANE('',#26866);
#1730=PLANE('',#26867);
#1731=PLANE('',#26869);
#1732=PLANE('',#26870);
#1733=PLANE('',#26872);
#1734=PLANE('',#26873);
#1735=PLANE('',#26875);
#1736=PLANE('',#26876);
#1737=PLANE('',#26877);
#1738=PLANE('',#26878);
#1739=PLANE('',#26879);
#1740=PLANE('',#26880);
#1741=PLANE('',#26881);
#1742=PLANE('',#26882);
#1743=PLANE('',#26891);
#1744=PLANE('',#26897);
#1745=PLANE('',#26899);
#1746=PLANE('',#26907);
#1747=FACE_OUTER_BOUND('',#3078,.T.);
#1748=FACE_OUTER_BOUND('',#3079,.T.);
#1749=FACE_OUTER_BOUND('',#3081,.T.);
#1750=FACE_OUTER_BOUND('',#3082,.T.);
#1751=FACE_OUTER_BOUND('',#3083,.T.);
#1752=FACE_OUTER_BOUND('',#3085,.T.);
#1753=FACE_OUTER_BOUND('',#3086,.T.);
#1754=FACE_OUTER_BOUND('',#3087,.T.);
#1755=FACE_OUTER_BOUND('',#3088,.T.);
#1756=FACE_OUTER_BOUND('',#3090,.T.);
#1757=FACE_OUTER_BOUND('',#3091,.T.);
#1758=FACE_OUTER_BOUND('',#3093,.T.);
#1759=FACE_OUTER_BOUND('',#3094,.T.);
#1760=FACE_OUTER_BOUND('',#3095,.T.);
#1761=FACE_OUTER_BOUND('',#3096,.T.);
#1762=FACE_OUTER_BOUND('',#3103,.T.);
#1763=FACE_OUTER_BOUND('',#3104,.T.);
#1764=FACE_OUTER_BOUND('',#3105,.T.);
#1765=FACE_OUTER_BOUND('',#3106,.T.);
#1766=FACE_OUTER_BOUND('',#3107,.T.);
#1767=FACE_OUTER_BOUND('',#3108,.T.);
#1768=FACE_OUTER_BOUND('',#3109,.T.);
#1769=FACE_OUTER_BOUND('',#3110,.T.);
#1770=FACE_OUTER_BOUND('',#3111,.T.);
#1771=FACE_OUTER_BOUND('',#3112,.T.);
#1772=FACE_OUTER_BOUND('',#3113,.T.);
#1773=FACE_OUTER_BOUND('',#3114,.T.);
#1774=FACE_OUTER_BOUND('',#3115,.T.);
#1775=FACE_OUTER_BOUND('',#3116,.T.);
#1776=FACE_OUTER_BOUND('',#3117,.T.);
#1777=FACE_OUTER_BOUND('',#3118,.T.);
#1778=FACE_OUTER_BOUND('',#3119,.T.);
#1779=FACE_OUTER_BOUND('',#3120,.T.);
#1780=FACE_OUTER_BOUND('',#3121,.T.);
#1781=FACE_OUTER_BOUND('',#3131,.T.);
#1782=FACE_OUTER_BOUND('',#3132,.T.);
#1783=FACE_OUTER_BOUND('',#3133,.T.);
#1784=FACE_OUTER_BOUND('',#3134,.T.);
#1785=FACE_OUTER_BOUND('',#3135,.T.);
#1786=FACE_OUTER_BOUND('',#3136,.T.);
#1787=FACE_OUTER_BOUND('',#3137,.T.);
#1788=FACE_OUTER_BOUND('',#3138,.T.);
#1789=FACE_OUTER_BOUND('',#3139,.T.);
#1790=FACE_OUTER_BOUND('',#3140,.T.);
#1791=FACE_OUTER_BOUND('',#3141,.T.);
#1792=FACE_OUTER_BOUND('',#3142,.T.);
#1793=FACE_OUTER_BOUND('',#3143,.T.);
#1794=FACE_OUTER_BOUND('',#3144,.T.);
#1795=FACE_OUTER_BOUND('',#3145,.T.);
#1796=FACE_OUTER_BOUND('',#3146,.T.);
#1797=FACE_OUTER_BOUND('',#3147,.T.);
#1798=FACE_OUTER_BOUND('',#3148,.T.);
#1799=FACE_OUTER_BOUND('',#3149,.T.);
#1800=FACE_OUTER_BOUND('',#3150,.T.);
#1801=FACE_OUTER_BOUND('',#3151,.T.);
#1802=FACE_OUTER_BOUND('',#3152,.T.);
#1803=FACE_OUTER_BOUND('',#3153,.T.);
#1804=FACE_OUTER_BOUND('',#3154,.T.);
#1805=FACE_OUTER_BOUND('',#3155,.T.);
#1806=FACE_OUTER_BOUND('',#3156,.T.);
#1807=FACE_OUTER_BOUND('',#3157,.T.);
#1808=FACE_OUTER_BOUND('',#3158,.T.);
#1809=FACE_OUTER_BOUND('',#3159,.T.);
#1810=FACE_OUTER_BOUND('',#3160,.T.);
#1811=FACE_OUTER_BOUND('',#3161,.T.);
#1812=FACE_OUTER_BOUND('',#3162,.T.);
#1813=FACE_OUTER_BOUND('',#3163,.T.);
#1814=FACE_OUTER_BOUND('',#3164,.T.);
#1815=FACE_OUTER_BOUND('',#3165,.T.);
#1816=FACE_OUTER_BOUND('',#3166,.T.);
#1817=FACE_OUTER_BOUND('',#3167,.T.);
#1818=FACE_OUTER_BOUND('',#3168,.T.);
#1819=FACE_OUTER_BOUND('',#3169,.T.);
#1820=FACE_OUTER_BOUND('',#3170,.T.);
#1821=FACE_OUTER_BOUND('',#3171,.T.);
#1822=FACE_OUTER_BOUND('',#3172,.T.);
#1823=FACE_OUTER_BOUND('',#3173,.T.);
#1824=FACE_OUTER_BOUND('',#3174,.T.);
#1825=FACE_OUTER_BOUND('',#3175,.T.);
#1826=FACE_OUTER_BOUND('',#3176,.T.);
#1827=FACE_OUTER_BOUND('',#3177,.T.);
#1828=FACE_OUTER_BOUND('',#3178,.T.);
#1829=FACE_OUTER_BOUND('',#3179,.T.);
#1830=FACE_OUTER_BOUND('',#3180,.T.);
#1831=FACE_OUTER_BOUND('',#3181,.T.);
#1832=FACE_OUTER_BOUND('',#3182,.T.);
#1833=FACE_OUTER_BOUND('',#3183,.T.);
#1834=FACE_OUTER_BOUND('',#3184,.T.);
#1835=FACE_OUTER_BOUND('',#3185,.T.);
#1836=FACE_OUTER_BOUND('',#3186,.T.);
#1837=FACE_OUTER_BOUND('',#3187,.T.);
#1838=FACE_OUTER_BOUND('',#3188,.T.);
#1839=FACE_OUTER_BOUND('',#3189,.T.);
#1840=FACE_OUTER_BOUND('',#3190,.T.);
#1841=FACE_OUTER_BOUND('',#3191,.T.);
#1842=FACE_OUTER_BOUND('',#3192,.T.);
#1843=FACE_OUTER_BOUND('',#3193,.T.);
#1844=FACE_OUTER_BOUND('',#3194,.T.);
#1845=FACE_OUTER_BOUND('',#3195,.T.);
#1846=FACE_OUTER_BOUND('',#3196,.T.);
#1847=FACE_OUTER_BOUND('',#3197,.T.);
#1848=FACE_OUTER_BOUND('',#3198,.T.);
#1849=FACE_OUTER_BOUND('',#3199,.T.);
#1850=FACE_OUTER_BOUND('',#3200,.T.);
#1851=FACE_OUTER_BOUND('',#3201,.T.);
#1852=FACE_OUTER_BOUND('',#3202,.T.);
#1853=FACE_OUTER_BOUND('',#3203,.T.);
#1854=FACE_OUTER_BOUND('',#3204,.T.);
#1855=FACE_OUTER_BOUND('',#3205,.T.);
#1856=FACE_OUTER_BOUND('',#3206,.T.);
#1857=FACE_OUTER_BOUND('',#3207,.T.);
#1858=FACE_OUTER_BOUND('',#3208,.T.);
#1859=FACE_OUTER_BOUND('',#3209,.T.);
#1860=FACE_OUTER_BOUND('',#3210,.T.);
#1861=FACE_OUTER_BOUND('',#3211,.T.);
#1862=FACE_OUTER_BOUND('',#3212,.T.);
#1863=FACE_OUTER_BOUND('',#3213,.T.);
#1864=FACE_OUTER_BOUND('',#3214,.T.);
#1865=FACE_OUTER_BOUND('',#3215,.T.);
#1866=FACE_OUTER_BOUND('',#3216,.T.);
#1867=FACE_OUTER_BOUND('',#3217,.T.);
#1868=FACE_OUTER_BOUND('',#3218,.T.);
#1869=FACE_OUTER_BOUND('',#3219,.T.);
#1870=FACE_OUTER_BOUND('',#3220,.T.);
#1871=FACE_OUTER_BOUND('',#3221,.T.);
#1872=FACE_OUTER_BOUND('',#3222,.T.);
#1873=FACE_OUTER_BOUND('',#3223,.T.);
#1874=FACE_OUTER_BOUND('',#3224,.T.);
#1875=FACE_OUTER_BOUND('',#3225,.T.);
#1876=FACE_OUTER_BOUND('',#3226,.T.);
#1877=FACE_OUTER_BOUND('',#3227,.T.);
#1878=FACE_OUTER_BOUND('',#3229,.T.);
#1879=FACE_OUTER_BOUND('',#3230,.T.);
#1880=FACE_OUTER_BOUND('',#3231,.T.);
#1881=FACE_OUTER_BOUND('',#3232,.T.);
#1882=FACE_OUTER_BOUND('',#3233,.T.);
#1883=FACE_OUTER_BOUND('',#3234,.T.);
#1884=FACE_OUTER_BOUND('',#3235,.T.);
#1885=FACE_OUTER_BOUND('',#3236,.T.);
#1886=FACE_OUTER_BOUND('',#3237,.T.);
#1887=FACE_OUTER_BOUND('',#3238,.T.);
#1888=FACE_OUTER_BOUND('',#3239,.T.);
#1889=FACE_OUTER_BOUND('',#3240,.T.);
#1890=FACE_OUTER_BOUND('',#3241,.T.);
#1891=FACE_OUTER_BOUND('',#3242,.T.);
#1892=FACE_OUTER_BOUND('',#3243,.T.);
#1893=FACE_OUTER_BOUND('',#3244,.T.);
#1894=FACE_OUTER_BOUND('',#3245,.T.);
#1895=FACE_OUTER_BOUND('',#3246,.T.);
#1896=FACE_OUTER_BOUND('',#3247,.T.);
#1897=FACE_OUTER_BOUND('',#3248,.T.);
#1898=FACE_OUTER_BOUND('',#3249,.T.);
#1899=FACE_OUTER_BOUND('',#3250,.T.);
#1900=FACE_OUTER_BOUND('',#3251,.T.);
#1901=FACE_OUTER_BOUND('',#3252,.T.);
#1902=FACE_OUTER_BOUND('',#3253,.T.);
#1903=FACE_OUTER_BOUND('',#3255,.T.);
#1904=FACE_OUTER_BOUND('',#3256,.T.);
#1905=FACE_OUTER_BOUND('',#3257,.T.);
#1906=FACE_OUTER_BOUND('',#3258,.T.);
#1907=FACE_OUTER_BOUND('',#3259,.T.);
#1908=FACE_OUTER_BOUND('',#3261,.T.);
#1909=FACE_OUTER_BOUND('',#3262,.T.);
#1910=FACE_OUTER_BOUND('',#3264,.T.);
#1911=FACE_OUTER_BOUND('',#3265,.T.);
#1912=FACE_OUTER_BOUND('',#3266,.T.);
#1913=FACE_OUTER_BOUND('',#3269,.T.);
#1914=FACE_OUTER_BOUND('',#3270,.T.);
#1915=FACE_OUTER_BOUND('',#3271,.T.);
#1916=FACE_OUTER_BOUND('',#3272,.T.);
#1917=FACE_OUTER_BOUND('',#3273,.T.);
#1918=FACE_OUTER_BOUND('',#3274,.T.);
#1919=FACE_OUTER_BOUND('',#3275,.T.);
#1920=FACE_OUTER_BOUND('',#3276,.T.);
#1921=FACE_OUTER_BOUND('',#3277,.T.);
#1922=FACE_OUTER_BOUND('',#3278,.T.);
#1923=FACE_OUTER_BOUND('',#3279,.T.);
#1924=FACE_OUTER_BOUND('',#3280,.T.);
#1925=FACE_OUTER_BOUND('',#3281,.T.);
#1926=FACE_OUTER_BOUND('',#3283,.T.);
#1927=FACE_OUTER_BOUND('',#3284,.T.);
#1928=FACE_OUTER_BOUND('',#3285,.T.);
#1929=FACE_OUTER_BOUND('',#3287,.T.);
#1930=FACE_OUTER_BOUND('',#3288,.T.);
#1931=FACE_OUTER_BOUND('',#3289,.T.);
#1932=FACE_OUTER_BOUND('',#3290,.T.);
#1933=FACE_OUTER_BOUND('',#3291,.T.);
#1934=FACE_OUTER_BOUND('',#3292,.T.);
#1935=FACE_OUTER_BOUND('',#3293,.T.);
#1936=FACE_OUTER_BOUND('',#3294,.T.);
#1937=FACE_OUTER_BOUND('',#3295,.T.);
#1938=FACE_OUTER_BOUND('',#3296,.T.);
#1939=FACE_OUTER_BOUND('',#3297,.T.);
#1940=FACE_OUTER_BOUND('',#3298,.T.);
#1941=FACE_OUTER_BOUND('',#3300,.T.);
#1942=FACE_OUTER_BOUND('',#3308,.T.);
#1943=FACE_OUTER_BOUND('',#3309,.T.);
#1944=FACE_OUTER_BOUND('',#3310,.T.);
#1945=FACE_OUTER_BOUND('',#3311,.T.);
#1946=FACE_OUTER_BOUND('',#3312,.T.);
#1947=FACE_OUTER_BOUND('',#3313,.T.);
#1948=FACE_OUTER_BOUND('',#3314,.T.);
#1949=FACE_OUTER_BOUND('',#3315,.T.);
#1950=FACE_OUTER_BOUND('',#3316,.T.);
#1951=FACE_OUTER_BOUND('',#3317,.T.);
#1952=FACE_OUTER_BOUND('',#3318,.T.);
#1953=FACE_OUTER_BOUND('',#3319,.T.);
#1954=FACE_OUTER_BOUND('',#3327,.T.);
#1955=FACE_OUTER_BOUND('',#3328,.T.);
#1956=FACE_OUTER_BOUND('',#3329,.T.);
#1957=FACE_OUTER_BOUND('',#3330,.T.);
#1958=FACE_OUTER_BOUND('',#3331,.T.);
#1959=FACE_OUTER_BOUND('',#3332,.T.);
#1960=FACE_OUTER_BOUND('',#3333,.T.);
#1961=FACE_OUTER_BOUND('',#3334,.T.);
#1962=FACE_OUTER_BOUND('',#3335,.T.);
#1963=FACE_OUTER_BOUND('',#3336,.T.);
#1964=FACE_OUTER_BOUND('',#3337,.T.);
#1965=FACE_OUTER_BOUND('',#3338,.T.);
#1966=FACE_OUTER_BOUND('',#3339,.T.);
#1967=FACE_OUTER_BOUND('',#3340,.T.);
#1968=FACE_OUTER_BOUND('',#3341,.T.);
#1969=FACE_OUTER_BOUND('',#3343,.T.);
#1970=FACE_OUTER_BOUND('',#3344,.T.);
#1971=FACE_OUTER_BOUND('',#3345,.T.);
#1972=FACE_OUTER_BOUND('',#3346,.T.);
#1973=FACE_OUTER_BOUND('',#3348,.T.);
#1974=FACE_OUTER_BOUND('',#3349,.T.);
#1975=FACE_OUTER_BOUND('',#3351,.T.);
#1976=FACE_OUTER_BOUND('',#3352,.T.);
#1977=FACE_OUTER_BOUND('',#3354,.T.);
#1978=FACE_OUTER_BOUND('',#3355,.T.);
#1979=FACE_OUTER_BOUND('',#3356,.T.);
#1980=FACE_OUTER_BOUND('',#3357,.T.);
#1981=FACE_OUTER_BOUND('',#3358,.T.);
#1982=FACE_OUTER_BOUND('',#3359,.T.);
#1983=FACE_OUTER_BOUND('',#3360,.T.);
#1984=FACE_OUTER_BOUND('',#3361,.T.);
#1985=FACE_OUTER_BOUND('',#3369,.T.);
#1986=FACE_OUTER_BOUND('',#3370,.T.);
#1987=FACE_OUTER_BOUND('',#3371,.T.);
#1988=FACE_OUTER_BOUND('',#3372,.T.);
#1989=FACE_OUTER_BOUND('',#3373,.T.);
#1990=FACE_OUTER_BOUND('',#3374,.T.);
#1991=FACE_OUTER_BOUND('',#3375,.T.);
#1992=FACE_OUTER_BOUND('',#3376,.T.);
#1993=FACE_OUTER_BOUND('',#3377,.T.);
#1994=FACE_OUTER_BOUND('',#3378,.T.);
#1995=FACE_OUTER_BOUND('',#3379,.T.);
#1996=FACE_OUTER_BOUND('',#3380,.T.);
#1997=FACE_OUTER_BOUND('',#3381,.T.);
#1998=FACE_OUTER_BOUND('',#3382,.T.);
#1999=FACE_OUTER_BOUND('',#3383,.T.);
#2000=FACE_OUTER_BOUND('',#3384,.T.);
#2001=FACE_OUTER_BOUND('',#3385,.T.);
#2002=FACE_OUTER_BOUND('',#3386,.T.);
#2003=FACE_OUTER_BOUND('',#3387,.T.);
#2004=FACE_OUTER_BOUND('',#3388,.T.);
#2005=FACE_OUTER_BOUND('',#3389,.T.);
#2006=FACE_OUTER_BOUND('',#3390,.T.);
#2007=FACE_OUTER_BOUND('',#3391,.T.);
#2008=FACE_OUTER_BOUND('',#3392,.T.);
#2009=FACE_OUTER_BOUND('',#3393,.T.);
#2010=FACE_OUTER_BOUND('',#3394,.T.);
#2011=FACE_OUTER_BOUND('',#3395,.T.);
#2012=FACE_OUTER_BOUND('',#3396,.T.);
#2013=FACE_OUTER_BOUND('',#3397,.T.);
#2014=FACE_OUTER_BOUND('',#3398,.T.);
#2015=FACE_OUTER_BOUND('',#3399,.T.);
#2016=FACE_OUTER_BOUND('',#3400,.T.);
#2017=FACE_OUTER_BOUND('',#3401,.T.);
#2018=FACE_OUTER_BOUND('',#3402,.T.);
#2019=FACE_OUTER_BOUND('',#3403,.T.);
#2020=FACE_OUTER_BOUND('',#3404,.T.);
#2021=FACE_OUTER_BOUND('',#3405,.T.);
#2022=FACE_OUTER_BOUND('',#3406,.T.);
#2023=FACE_OUTER_BOUND('',#3407,.T.);
#2024=FACE_OUTER_BOUND('',#3408,.T.);
#2025=FACE_OUTER_BOUND('',#3409,.T.);
#2026=FACE_OUTER_BOUND('',#3410,.T.);
#2027=FACE_OUTER_BOUND('',#3411,.T.);
#2028=FACE_OUTER_BOUND('',#3412,.T.);
#2029=FACE_OUTER_BOUND('',#3414,.T.);
#2030=FACE_OUTER_BOUND('',#3415,.T.);
#2031=FACE_OUTER_BOUND('',#3416,.T.);
#2032=FACE_OUTER_BOUND('',#3417,.T.);
#2033=FACE_OUTER_BOUND('',#3418,.T.);
#2034=FACE_OUTER_BOUND('',#3420,.T.);
#2035=FACE_OUTER_BOUND('',#3421,.T.);
#2036=FACE_OUTER_BOUND('',#3422,.T.);
#2037=FACE_OUTER_BOUND('',#3423,.T.);
#2038=FACE_OUTER_BOUND('',#3424,.T.);
#2039=FACE_OUTER_BOUND('',#3425,.T.);
#2040=FACE_OUTER_BOUND('',#3426,.T.);
#2041=FACE_OUTER_BOUND('',#3427,.T.);
#2042=FACE_OUTER_BOUND('',#3428,.T.);
#2043=FACE_OUTER_BOUND('',#3429,.T.);
#2044=FACE_OUTER_BOUND('',#3430,.T.);
#2045=FACE_OUTER_BOUND('',#3432,.T.);
#2046=FACE_OUTER_BOUND('',#3434,.T.);
#2047=FACE_OUTER_BOUND('',#3436,.T.);
#2048=FACE_OUTER_BOUND('',#3438,.T.);
#2049=FACE_OUTER_BOUND('',#3439,.T.);
#2050=FACE_OUTER_BOUND('',#3440,.T.);
#2051=FACE_OUTER_BOUND('',#3441,.T.);
#2052=FACE_OUTER_BOUND('',#3442,.T.);
#2053=FACE_OUTER_BOUND('',#3443,.T.);
#2054=FACE_OUTER_BOUND('',#3445,.T.);
#2055=FACE_OUTER_BOUND('',#3446,.T.);
#2056=FACE_OUTER_BOUND('',#3447,.T.);
#2057=FACE_OUTER_BOUND('',#3448,.T.);
#2058=FACE_OUTER_BOUND('',#3449,.T.);
#2059=FACE_OUTER_BOUND('',#3450,.T.);
#2060=FACE_OUTER_BOUND('',#3451,.T.);
#2061=FACE_OUTER_BOUND('',#3452,.T.);
#2062=FACE_OUTER_BOUND('',#3453,.T.);
#2063=FACE_OUTER_BOUND('',#3454,.T.);
#2064=FACE_OUTER_BOUND('',#3455,.T.);
#2065=FACE_OUTER_BOUND('',#3456,.T.);
#2066=FACE_OUTER_BOUND('',#3457,.T.);
#2067=FACE_OUTER_BOUND('',#3458,.T.);
#2068=FACE_OUTER_BOUND('',#3459,.T.);
#2069=FACE_OUTER_BOUND('',#3460,.T.);
#2070=FACE_OUTER_BOUND('',#3461,.T.);
#2071=FACE_OUTER_BOUND('',#3462,.T.);
#2072=FACE_OUTER_BOUND('',#3463,.T.);
#2073=FACE_OUTER_BOUND('',#3464,.T.);
#2074=FACE_OUTER_BOUND('',#3465,.T.);
#2075=FACE_OUTER_BOUND('',#3466,.T.);
#2076=FACE_OUTER_BOUND('',#3467,.T.);
#2077=FACE_OUTER_BOUND('',#3468,.T.);
#2078=FACE_OUTER_BOUND('',#3469,.T.);
#2079=FACE_OUTER_BOUND('',#3470,.T.);
#2080=FACE_OUTER_BOUND('',#3471,.T.);
#2081=FACE_OUTER_BOUND('',#3472,.T.);
#2082=FACE_OUTER_BOUND('',#3473,.T.);
#2083=FACE_OUTER_BOUND('',#3474,.T.);
#2084=FACE_OUTER_BOUND('',#3475,.T.);
#2085=FACE_OUTER_BOUND('',#3476,.T.);
#2086=FACE_OUTER_BOUND('',#3477,.T.);
#2087=FACE_OUTER_BOUND('',#3478,.T.);
#2088=FACE_OUTER_BOUND('',#3479,.T.);
#2089=FACE_OUTER_BOUND('',#3480,.T.);
#2090=FACE_OUTER_BOUND('',#3481,.T.);
#2091=FACE_OUTER_BOUND('',#3482,.T.);
#2092=FACE_OUTER_BOUND('',#3483,.T.);
#2093=FACE_OUTER_BOUND('',#3484,.T.);
#2094=FACE_OUTER_BOUND('',#3485,.T.);
#2095=FACE_OUTER_BOUND('',#3486,.T.);
#2096=FACE_OUTER_BOUND('',#3487,.T.);
#2097=FACE_OUTER_BOUND('',#3488,.T.);
#2098=FACE_OUTER_BOUND('',#3489,.T.);
#2099=FACE_OUTER_BOUND('',#3490,.T.);
#2100=FACE_OUTER_BOUND('',#3491,.T.);
#2101=FACE_OUTER_BOUND('',#3492,.T.);
#2102=FACE_OUTER_BOUND('',#3493,.T.);
#2103=FACE_OUTER_BOUND('',#3494,.T.);
#2104=FACE_OUTER_BOUND('',#3495,.T.);
#2105=FACE_OUTER_BOUND('',#3496,.T.);
#2106=FACE_OUTER_BOUND('',#3497,.T.);
#2107=FACE_OUTER_BOUND('',#3498,.T.);
#2108=FACE_OUTER_BOUND('',#3499,.T.);
#2109=FACE_OUTER_BOUND('',#3500,.T.);
#2110=FACE_OUTER_BOUND('',#3501,.T.);
#2111=FACE_OUTER_BOUND('',#3502,.T.);
#2112=FACE_OUTER_BOUND('',#3503,.T.);
#2113=FACE_OUTER_BOUND('',#3504,.T.);
#2114=FACE_OUTER_BOUND('',#3505,.T.);
#2115=FACE_OUTER_BOUND('',#3506,.T.);
#2116=FACE_OUTER_BOUND('',#3507,.T.);
#2117=FACE_OUTER_BOUND('',#3508,.T.);
#2118=FACE_OUTER_BOUND('',#3509,.T.);
#2119=FACE_OUTER_BOUND('',#3510,.T.);
#2120=FACE_OUTER_BOUND('',#3511,.T.);
#2121=FACE_OUTER_BOUND('',#3512,.T.);
#2122=FACE_OUTER_BOUND('',#3513,.T.);
#2123=FACE_OUTER_BOUND('',#3514,.T.);
#2124=FACE_OUTER_BOUND('',#3515,.T.);
#2125=FACE_OUTER_BOUND('',#3516,.T.);
#2126=FACE_OUTER_BOUND('',#3517,.T.);
#2127=FACE_OUTER_BOUND('',#3519,.T.);
#2128=FACE_OUTER_BOUND('',#3520,.T.);
#2129=FACE_OUTER_BOUND('',#3521,.T.);
#2130=FACE_OUTER_BOUND('',#3522,.T.);
#2131=FACE_OUTER_BOUND('',#3523,.T.);
#2132=FACE_OUTER_BOUND('',#3524,.T.);
#2133=FACE_OUTER_BOUND('',#3525,.T.);
#2134=FACE_OUTER_BOUND('',#3526,.T.);
#2135=FACE_OUTER_BOUND('',#3527,.T.);
#2136=FACE_OUTER_BOUND('',#3528,.T.);
#2137=FACE_OUTER_BOUND('',#3529,.T.);
#2138=FACE_OUTER_BOUND('',#3530,.T.);
#2139=FACE_OUTER_BOUND('',#3531,.T.);
#2140=FACE_OUTER_BOUND('',#3532,.T.);
#2141=FACE_OUTER_BOUND('',#3533,.T.);
#2142=FACE_OUTER_BOUND('',#3534,.T.);
#2143=FACE_OUTER_BOUND('',#3535,.T.);
#2144=FACE_OUTER_BOUND('',#3536,.T.);
#2145=FACE_OUTER_BOUND('',#3537,.T.);
#2146=FACE_OUTER_BOUND('',#3538,.T.);
#2147=FACE_OUTER_BOUND('',#3539,.T.);
#2148=FACE_OUTER_BOUND('',#3540,.T.);
#2149=FACE_OUTER_BOUND('',#3541,.T.);
#2150=FACE_OUTER_BOUND('',#3542,.T.);
#2151=FACE_OUTER_BOUND('',#3543,.T.);
#2152=FACE_OUTER_BOUND('',#3544,.T.);
#2153=FACE_OUTER_BOUND('',#3545,.T.);
#2154=FACE_OUTER_BOUND('',#3546,.T.);
#2155=FACE_OUTER_BOUND('',#3547,.T.);
#2156=FACE_OUTER_BOUND('',#3548,.T.);
#2157=FACE_OUTER_BOUND('',#3549,.T.);
#2158=FACE_OUTER_BOUND('',#3550,.T.);
#2159=FACE_OUTER_BOUND('',#3551,.T.);
#2160=FACE_OUTER_BOUND('',#3552,.T.);
#2161=FACE_OUTER_BOUND('',#3553,.T.);
#2162=FACE_OUTER_BOUND('',#3554,.T.);
#2163=FACE_OUTER_BOUND('',#3555,.T.);
#2164=FACE_OUTER_BOUND('',#3556,.T.);
#2165=FACE_OUTER_BOUND('',#3557,.T.);
#2166=FACE_OUTER_BOUND('',#3558,.T.);
#2167=FACE_OUTER_BOUND('',#3559,.T.);
#2168=FACE_OUTER_BOUND('',#3560,.T.);
#2169=FACE_OUTER_BOUND('',#3561,.T.);
#2170=FACE_OUTER_BOUND('',#3562,.T.);
#2171=FACE_OUTER_BOUND('',#3563,.T.);
#2172=FACE_OUTER_BOUND('',#3564,.T.);
#2173=FACE_OUTER_BOUND('',#3565,.T.);
#2174=FACE_OUTER_BOUND('',#3566,.T.);
#2175=FACE_OUTER_BOUND('',#3567,.T.);
#2176=FACE_OUTER_BOUND('',#3568,.T.);
#2177=FACE_OUTER_BOUND('',#3569,.T.);
#2178=FACE_OUTER_BOUND('',#3570,.T.);
#2179=FACE_OUTER_BOUND('',#3571,.T.);
#2180=FACE_OUTER_BOUND('',#3572,.T.);
#2181=FACE_OUTER_BOUND('',#3573,.T.);
#2182=FACE_OUTER_BOUND('',#3574,.T.);
#2183=FACE_OUTER_BOUND('',#3575,.T.);
#2184=FACE_OUTER_BOUND('',#3576,.T.);
#2185=FACE_OUTER_BOUND('',#3577,.T.);
#2186=FACE_OUTER_BOUND('',#3578,.T.);
#2187=FACE_OUTER_BOUND('',#3579,.T.);
#2188=FACE_OUTER_BOUND('',#3580,.T.);
#2189=FACE_OUTER_BOUND('',#3581,.T.);
#2190=FACE_OUTER_BOUND('',#3582,.T.);
#2191=FACE_OUTER_BOUND('',#3583,.T.);
#2192=FACE_OUTER_BOUND('',#3584,.T.);
#2193=FACE_OUTER_BOUND('',#3585,.T.);
#2194=FACE_OUTER_BOUND('',#3586,.T.);
#2195=FACE_OUTER_BOUND('',#3587,.T.);
#2196=FACE_OUTER_BOUND('',#3588,.T.);
#2197=FACE_OUTER_BOUND('',#3589,.T.);
#2198=FACE_OUTER_BOUND('',#3590,.T.);
#2199=FACE_OUTER_BOUND('',#3591,.T.);
#2200=FACE_OUTER_BOUND('',#3592,.T.);
#2201=FACE_OUTER_BOUND('',#3593,.T.);
#2202=FACE_OUTER_BOUND('',#3594,.T.);
#2203=FACE_OUTER_BOUND('',#3595,.T.);
#2204=FACE_OUTER_BOUND('',#3596,.T.);
#2205=FACE_OUTER_BOUND('',#3597,.T.);
#2206=FACE_OUTER_BOUND('',#3598,.T.);
#2207=FACE_OUTER_BOUND('',#3599,.T.);
#2208=FACE_OUTER_BOUND('',#3600,.T.);
#2209=FACE_OUTER_BOUND('',#3601,.T.);
#2210=FACE_OUTER_BOUND('',#3602,.T.);
#2211=FACE_OUTER_BOUND('',#3603,.T.);
#2212=FACE_OUTER_BOUND('',#3604,.T.);
#2213=FACE_OUTER_BOUND('',#3605,.T.);
#2214=FACE_OUTER_BOUND('',#3606,.T.);
#2215=FACE_OUTER_BOUND('',#3607,.T.);
#2216=FACE_OUTER_BOUND('',#3608,.T.);
#2217=FACE_OUTER_BOUND('',#3609,.T.);
#2218=FACE_OUTER_BOUND('',#3610,.T.);
#2219=FACE_OUTER_BOUND('',#3611,.T.);
#2220=FACE_OUTER_BOUND('',#3612,.T.);
#2221=FACE_OUTER_BOUND('',#3613,.T.);
#2222=FACE_OUTER_BOUND('',#3614,.T.);
#2223=FACE_OUTER_BOUND('',#3615,.T.);
#2224=FACE_OUTER_BOUND('',#3616,.T.);
#2225=FACE_OUTER_BOUND('',#3617,.T.);
#2226=FACE_OUTER_BOUND('',#3618,.T.);
#2227=FACE_OUTER_BOUND('',#3619,.T.);
#2228=FACE_OUTER_BOUND('',#3620,.T.);
#2229=FACE_OUTER_BOUND('',#3621,.T.);
#2230=FACE_OUTER_BOUND('',#3622,.T.);
#2231=FACE_OUTER_BOUND('',#3623,.T.);
#2232=FACE_OUTER_BOUND('',#3624,.T.);
#2233=FACE_OUTER_BOUND('',#3625,.T.);
#2234=FACE_OUTER_BOUND('',#3626,.T.);
#2235=FACE_OUTER_BOUND('',#3627,.T.);
#2236=FACE_OUTER_BOUND('',#3628,.T.);
#2237=FACE_OUTER_BOUND('',#3629,.T.);
#2238=FACE_OUTER_BOUND('',#3630,.T.);
#2239=FACE_OUTER_BOUND('',#3631,.T.);
#2240=FACE_OUTER_BOUND('',#3632,.T.);
#2241=FACE_OUTER_BOUND('',#3633,.T.);
#2242=FACE_OUTER_BOUND('',#3634,.T.);
#2243=FACE_OUTER_BOUND('',#3635,.T.);
#2244=FACE_OUTER_BOUND('',#3636,.T.);
#2245=FACE_OUTER_BOUND('',#3637,.T.);
#2246=FACE_OUTER_BOUND('',#3638,.T.);
#2247=FACE_OUTER_BOUND('',#3639,.T.);
#2248=FACE_OUTER_BOUND('',#3640,.T.);
#2249=FACE_OUTER_BOUND('',#3641,.T.);
#2250=FACE_OUTER_BOUND('',#3642,.T.);
#2251=FACE_OUTER_BOUND('',#3643,.T.);
#2252=FACE_OUTER_BOUND('',#3644,.T.);
#2253=FACE_OUTER_BOUND('',#3645,.T.);
#2254=FACE_OUTER_BOUND('',#3646,.T.);
#2255=FACE_OUTER_BOUND('',#3647,.T.);
#2256=FACE_OUTER_BOUND('',#3648,.T.);
#2257=FACE_OUTER_BOUND('',#3649,.T.);
#2258=FACE_OUTER_BOUND('',#3650,.T.);
#2259=FACE_OUTER_BOUND('',#3651,.T.);
#2260=FACE_OUTER_BOUND('',#3652,.T.);
#2261=FACE_OUTER_BOUND('',#3653,.T.);
#2262=FACE_OUTER_BOUND('',#3654,.T.);
#2263=FACE_OUTER_BOUND('',#3655,.T.);
#2264=FACE_OUTER_BOUND('',#3656,.T.);
#2265=FACE_OUTER_BOUND('',#3657,.T.);
#2266=FACE_OUTER_BOUND('',#3658,.T.);
#2267=FACE_OUTER_BOUND('',#3659,.T.);
#2268=FACE_OUTER_BOUND('',#3660,.T.);
#2269=FACE_OUTER_BOUND('',#3661,.T.);
#2270=FACE_OUTER_BOUND('',#3662,.T.);
#2271=FACE_OUTER_BOUND('',#3663,.T.);
#2272=FACE_OUTER_BOUND('',#3664,.T.);
#2273=FACE_OUTER_BOUND('',#3665,.T.);
#2274=FACE_OUTER_BOUND('',#3666,.T.);
#2275=FACE_OUTER_BOUND('',#3667,.T.);
#2276=FACE_OUTER_BOUND('',#3668,.T.);
#2277=FACE_OUTER_BOUND('',#3669,.T.);
#2278=FACE_OUTER_BOUND('',#3670,.T.);
#2279=FACE_OUTER_BOUND('',#3671,.T.);
#2280=FACE_OUTER_BOUND('',#3672,.T.);
#2281=FACE_OUTER_BOUND('',#3673,.T.);
#2282=FACE_OUTER_BOUND('',#3674,.T.);
#2283=FACE_OUTER_BOUND('',#3675,.T.);
#2284=FACE_OUTER_BOUND('',#3676,.T.);
#2285=FACE_OUTER_BOUND('',#3677,.T.);
#2286=FACE_OUTER_BOUND('',#3678,.T.);
#2287=FACE_OUTER_BOUND('',#3679,.T.);
#2288=FACE_OUTER_BOUND('',#3680,.T.);
#2289=FACE_OUTER_BOUND('',#3681,.T.);
#2290=FACE_OUTER_BOUND('',#3682,.T.);
#2291=FACE_OUTER_BOUND('',#3683,.T.);
#2292=FACE_OUTER_BOUND('',#3684,.T.);
#2293=FACE_OUTER_BOUND('',#3685,.T.);
#2294=FACE_OUTER_BOUND('',#3686,.T.);
#2295=FACE_OUTER_BOUND('',#3687,.T.);
#2296=FACE_OUTER_BOUND('',#3688,.T.);
#2297=FACE_OUTER_BOUND('',#3689,.T.);
#2298=FACE_OUTER_BOUND('',#3690,.T.);
#2299=FACE_OUTER_BOUND('',#3691,.T.);
#2300=FACE_OUTER_BOUND('',#3692,.T.);
#2301=FACE_OUTER_BOUND('',#3693,.T.);
#2302=FACE_OUTER_BOUND('',#3694,.T.);
#2303=FACE_OUTER_BOUND('',#3695,.T.);
#2304=FACE_OUTER_BOUND('',#3696,.T.);
#2305=FACE_OUTER_BOUND('',#3697,.T.);
#2306=FACE_OUTER_BOUND('',#3698,.T.);
#2307=FACE_OUTER_BOUND('',#3699,.T.);
#2308=FACE_OUTER_BOUND('',#3700,.T.);
#2309=FACE_OUTER_BOUND('',#3701,.T.);
#2310=FACE_OUTER_BOUND('',#3702,.T.);
#2311=FACE_OUTER_BOUND('',#3703,.T.);
#2312=FACE_OUTER_BOUND('',#3704,.T.);
#2313=FACE_OUTER_BOUND('',#3705,.T.);
#2314=FACE_OUTER_BOUND('',#3706,.T.);
#2315=FACE_OUTER_BOUND('',#3707,.T.);
#2316=FACE_OUTER_BOUND('',#3708,.T.);
#2317=FACE_OUTER_BOUND('',#3709,.T.);
#2318=FACE_OUTER_BOUND('',#3710,.T.);
#2319=FACE_OUTER_BOUND('',#3711,.T.);
#2320=FACE_OUTER_BOUND('',#3712,.T.);
#2321=FACE_OUTER_BOUND('',#3713,.T.);
#2322=FACE_OUTER_BOUND('',#3714,.T.);
#2323=FACE_OUTER_BOUND('',#3715,.T.);
#2324=FACE_OUTER_BOUND('',#3716,.T.);
#2325=FACE_OUTER_BOUND('',#3717,.T.);
#2326=FACE_OUTER_BOUND('',#3718,.T.);
#2327=FACE_OUTER_BOUND('',#3719,.T.);
#2328=FACE_OUTER_BOUND('',#3720,.T.);
#2329=FACE_OUTER_BOUND('',#3721,.T.);
#2330=FACE_OUTER_BOUND('',#3722,.T.);
#2331=FACE_OUTER_BOUND('',#3723,.T.);
#2332=FACE_OUTER_BOUND('',#3724,.T.);
#2333=FACE_OUTER_BOUND('',#3725,.T.);
#2334=FACE_OUTER_BOUND('',#3726,.T.);
#2335=FACE_OUTER_BOUND('',#3727,.T.);
#2336=FACE_OUTER_BOUND('',#3728,.T.);
#2337=FACE_OUTER_BOUND('',#3729,.T.);
#2338=FACE_OUTER_BOUND('',#3730,.T.);
#2339=FACE_OUTER_BOUND('',#3731,.T.);
#2340=FACE_OUTER_BOUND('',#3732,.T.);
#2341=FACE_OUTER_BOUND('',#3733,.T.);
#2342=FACE_OUTER_BOUND('',#3734,.T.);
#2343=FACE_OUTER_BOUND('',#3735,.T.);
#2344=FACE_OUTER_BOUND('',#3736,.T.);
#2345=FACE_OUTER_BOUND('',#3737,.T.);
#2346=FACE_OUTER_BOUND('',#3738,.T.);
#2347=FACE_OUTER_BOUND('',#3739,.T.);
#2348=FACE_OUTER_BOUND('',#3740,.T.);
#2349=FACE_OUTER_BOUND('',#3741,.T.);
#2350=FACE_OUTER_BOUND('',#3742,.T.);
#2351=FACE_OUTER_BOUND('',#3743,.T.);
#2352=FACE_OUTER_BOUND('',#3744,.T.);
#2353=FACE_OUTER_BOUND('',#3745,.T.);
#2354=FACE_OUTER_BOUND('',#3746,.T.);
#2355=FACE_OUTER_BOUND('',#3747,.T.);
#2356=FACE_OUTER_BOUND('',#3748,.T.);
#2357=FACE_OUTER_BOUND('',#3749,.T.);
#2358=FACE_OUTER_BOUND('',#3750,.T.);
#2359=FACE_OUTER_BOUND('',#3751,.T.);
#2360=FACE_OUTER_BOUND('',#3752,.T.);
#2361=FACE_OUTER_BOUND('',#3753,.T.);
#2362=FACE_OUTER_BOUND('',#3754,.T.);
#2363=FACE_OUTER_BOUND('',#3755,.T.);
#2364=FACE_OUTER_BOUND('',#3756,.T.);
#2365=FACE_OUTER_BOUND('',#3757,.T.);
#2366=FACE_OUTER_BOUND('',#3758,.T.);
#2367=FACE_OUTER_BOUND('',#3759,.T.);
#2368=FACE_OUTER_BOUND('',#3760,.T.);
#2369=FACE_OUTER_BOUND('',#3761,.T.);
#2370=FACE_OUTER_BOUND('',#3762,.T.);
#2371=FACE_OUTER_BOUND('',#3763,.T.);
#2372=FACE_OUTER_BOUND('',#3764,.T.);
#2373=FACE_OUTER_BOUND('',#3765,.T.);
#2374=FACE_OUTER_BOUND('',#3766,.T.);
#2375=FACE_OUTER_BOUND('',#3767,.T.);
#2376=FACE_OUTER_BOUND('',#3768,.T.);
#2377=FACE_OUTER_BOUND('',#3769,.T.);
#2378=FACE_OUTER_BOUND('',#3770,.T.);
#2379=FACE_OUTER_BOUND('',#3771,.T.);
#2380=FACE_OUTER_BOUND('',#3772,.T.);
#2381=FACE_OUTER_BOUND('',#3773,.T.);
#2382=FACE_OUTER_BOUND('',#3774,.T.);
#2383=FACE_OUTER_BOUND('',#3775,.T.);
#2384=FACE_OUTER_BOUND('',#3776,.T.);
#2385=FACE_OUTER_BOUND('',#3777,.T.);
#2386=FACE_OUTER_BOUND('',#3778,.T.);
#2387=FACE_OUTER_BOUND('',#3779,.T.);
#2388=FACE_OUTER_BOUND('',#3780,.T.);
#2389=FACE_OUTER_BOUND('',#3781,.T.);
#2390=FACE_OUTER_BOUND('',#3782,.T.);
#2391=FACE_OUTER_BOUND('',#3783,.T.);
#2392=FACE_OUTER_BOUND('',#3784,.T.);
#2393=FACE_OUTER_BOUND('',#3785,.T.);
#2394=FACE_OUTER_BOUND('',#3786,.T.);
#2395=FACE_OUTER_BOUND('',#3787,.T.);
#2396=FACE_OUTER_BOUND('',#3788,.T.);
#2397=FACE_OUTER_BOUND('',#3789,.T.);
#2398=FACE_OUTER_BOUND('',#3790,.T.);
#2399=FACE_OUTER_BOUND('',#3792,.T.);
#2400=FACE_OUTER_BOUND('',#3794,.T.);
#2401=FACE_OUTER_BOUND('',#3795,.T.);
#2402=FACE_OUTER_BOUND('',#3796,.T.);
#2403=FACE_OUTER_BOUND('',#3797,.T.);
#2404=FACE_OUTER_BOUND('',#3799,.T.);
#2405=FACE_OUTER_BOUND('',#3800,.T.);
#2406=FACE_OUTER_BOUND('',#3801,.T.);
#2407=FACE_OUTER_BOUND('',#3802,.T.);
#2408=FACE_OUTER_BOUND('',#3803,.T.);
#2409=FACE_OUTER_BOUND('',#3804,.T.);
#2410=FACE_OUTER_BOUND('',#3805,.T.);
#2411=FACE_OUTER_BOUND('',#3806,.T.);
#2412=FACE_OUTER_BOUND('',#3807,.T.);
#2413=FACE_OUTER_BOUND('',#3808,.T.);
#2414=FACE_OUTER_BOUND('',#3809,.T.);
#2415=FACE_OUTER_BOUND('',#3810,.T.);
#2416=FACE_OUTER_BOUND('',#3811,.T.);
#2417=FACE_OUTER_BOUND('',#3812,.T.);
#2418=FACE_OUTER_BOUND('',#3813,.T.);
#2419=FACE_OUTER_BOUND('',#3814,.T.);
#2420=FACE_OUTER_BOUND('',#3815,.T.);
#2421=FACE_OUTER_BOUND('',#3816,.T.);
#2422=FACE_OUTER_BOUND('',#3817,.T.);
#2423=FACE_OUTER_BOUND('',#3818,.T.);
#2424=FACE_OUTER_BOUND('',#3819,.T.);
#2425=FACE_OUTER_BOUND('',#3820,.T.);
#2426=FACE_OUTER_BOUND('',#3821,.T.);
#2427=FACE_OUTER_BOUND('',#3822,.T.);
#2428=FACE_OUTER_BOUND('',#3823,.T.);
#2429=FACE_OUTER_BOUND('',#3824,.T.);
#2430=FACE_OUTER_BOUND('',#3825,.T.);
#2431=FACE_OUTER_BOUND('',#3826,.T.);
#2432=FACE_OUTER_BOUND('',#3827,.T.);
#2433=FACE_OUTER_BOUND('',#3828,.T.);
#2434=FACE_OUTER_BOUND('',#3829,.T.);
#2435=FACE_OUTER_BOUND('',#3830,.T.);
#2436=FACE_OUTER_BOUND('',#3831,.T.);
#2437=FACE_OUTER_BOUND('',#3832,.T.);
#2438=FACE_OUTER_BOUND('',#3833,.T.);
#2439=FACE_OUTER_BOUND('',#3834,.T.);
#2440=FACE_OUTER_BOUND('',#3835,.T.);
#2441=FACE_OUTER_BOUND('',#3836,.T.);
#2442=FACE_OUTER_BOUND('',#3837,.T.);
#2443=FACE_OUTER_BOUND('',#3838,.T.);
#2444=FACE_OUTER_BOUND('',#3839,.T.);
#2445=FACE_OUTER_BOUND('',#3840,.T.);
#2446=FACE_OUTER_BOUND('',#3841,.T.);
#2447=FACE_OUTER_BOUND('',#3842,.T.);
#2448=FACE_OUTER_BOUND('',#3843,.T.);
#2449=FACE_OUTER_BOUND('',#3844,.T.);
#2450=FACE_OUTER_BOUND('',#3845,.T.);
#2451=FACE_OUTER_BOUND('',#3846,.T.);
#2452=FACE_OUTER_BOUND('',#3847,.T.);
#2453=FACE_OUTER_BOUND('',#3848,.T.);
#2454=FACE_OUTER_BOUND('',#3849,.T.);
#2455=FACE_OUTER_BOUND('',#3850,.T.);
#2456=FACE_OUTER_BOUND('',#3851,.T.);
#2457=FACE_OUTER_BOUND('',#3852,.T.);
#2458=FACE_OUTER_BOUND('',#3853,.T.);
#2459=FACE_OUTER_BOUND('',#3854,.T.);
#2460=FACE_OUTER_BOUND('',#3855,.T.);
#2461=FACE_OUTER_BOUND('',#3856,.T.);
#2462=FACE_OUTER_BOUND('',#3857,.T.);
#2463=FACE_OUTER_BOUND('',#3858,.T.);
#2464=FACE_OUTER_BOUND('',#3859,.T.);
#2465=FACE_OUTER_BOUND('',#3860,.T.);
#2466=FACE_OUTER_BOUND('',#3861,.T.);
#2467=FACE_OUTER_BOUND('',#3862,.T.);
#2468=FACE_OUTER_BOUND('',#3863,.T.);
#2469=FACE_OUTER_BOUND('',#3864,.T.);
#2470=FACE_OUTER_BOUND('',#3865,.T.);
#2471=FACE_OUTER_BOUND('',#3866,.T.);
#2472=FACE_OUTER_BOUND('',#3867,.T.);
#2473=FACE_OUTER_BOUND('',#3868,.T.);
#2474=FACE_OUTER_BOUND('',#3869,.T.);
#2475=FACE_OUTER_BOUND('',#3870,.T.);
#2476=FACE_OUTER_BOUND('',#3871,.T.);
#2477=FACE_OUTER_BOUND('',#3873,.T.);
#2478=FACE_OUTER_BOUND('',#3874,.T.);
#2479=FACE_OUTER_BOUND('',#3875,.T.);
#2480=FACE_OUTER_BOUND('',#3876,.T.);
#2481=FACE_OUTER_BOUND('',#3877,.T.);
#2482=FACE_OUTER_BOUND('',#3878,.T.);
#2483=FACE_OUTER_BOUND('',#3879,.T.);
#2484=FACE_OUTER_BOUND('',#3880,.T.);
#2485=FACE_OUTER_BOUND('',#3881,.T.);
#2486=FACE_OUTER_BOUND('',#3882,.T.);
#2487=FACE_OUTER_BOUND('',#3883,.T.);
#2488=FACE_OUTER_BOUND('',#3884,.T.);
#2489=FACE_OUTER_BOUND('',#3885,.T.);
#2490=FACE_OUTER_BOUND('',#3886,.T.);
#2491=FACE_OUTER_BOUND('',#3887,.T.);
#2492=FACE_OUTER_BOUND('',#3888,.T.);
#2493=FACE_OUTER_BOUND('',#3889,.T.);
#2494=FACE_OUTER_BOUND('',#3890,.T.);
#2495=FACE_OUTER_BOUND('',#3891,.T.);
#2496=FACE_OUTER_BOUND('',#3892,.T.);
#2497=FACE_OUTER_BOUND('',#3893,.T.);
#2498=FACE_OUTER_BOUND('',#3894,.T.);
#2499=FACE_OUTER_BOUND('',#3895,.T.);
#2500=FACE_OUTER_BOUND('',#3896,.T.);
#2501=FACE_OUTER_BOUND('',#3897,.T.);
#2502=FACE_OUTER_BOUND('',#3898,.T.);
#2503=FACE_OUTER_BOUND('',#3899,.T.);
#2504=FACE_OUTER_BOUND('',#3900,.T.);
#2505=FACE_OUTER_BOUND('',#3901,.T.);
#2506=FACE_OUTER_BOUND('',#3902,.T.);
#2507=FACE_OUTER_BOUND('',#3903,.T.);
#2508=FACE_OUTER_BOUND('',#3904,.T.);
#2509=FACE_OUTER_BOUND('',#3905,.T.);
#2510=FACE_OUTER_BOUND('',#3906,.T.);
#2511=FACE_OUTER_BOUND('',#3907,.T.);
#2512=FACE_OUTER_BOUND('',#3908,.T.);
#2513=FACE_OUTER_BOUND('',#3909,.T.);
#2514=FACE_OUTER_BOUND('',#3910,.T.);
#2515=FACE_OUTER_BOUND('',#3911,.T.);
#2516=FACE_OUTER_BOUND('',#3912,.T.);
#2517=FACE_OUTER_BOUND('',#3913,.T.);
#2518=FACE_OUTER_BOUND('',#3914,.T.);
#2519=FACE_OUTER_BOUND('',#3915,.T.);
#2520=FACE_OUTER_BOUND('',#3916,.T.);
#2521=FACE_OUTER_BOUND('',#3917,.T.);
#2522=FACE_OUTER_BOUND('',#3918,.T.);
#2523=FACE_OUTER_BOUND('',#3919,.T.);
#2524=FACE_OUTER_BOUND('',#3920,.T.);
#2525=FACE_OUTER_BOUND('',#3921,.T.);
#2526=FACE_OUTER_BOUND('',#3922,.T.);
#2527=FACE_OUTER_BOUND('',#3923,.T.);
#2528=FACE_OUTER_BOUND('',#3924,.T.);
#2529=FACE_OUTER_BOUND('',#3925,.T.);
#2530=FACE_OUTER_BOUND('',#3926,.T.);
#2531=FACE_OUTER_BOUND('',#3927,.T.);
#2532=FACE_OUTER_BOUND('',#3928,.T.);
#2533=FACE_OUTER_BOUND('',#3929,.T.);
#2534=FACE_OUTER_BOUND('',#3930,.T.);
#2535=FACE_OUTER_BOUND('',#3931,.T.);
#2536=FACE_OUTER_BOUND('',#3932,.T.);
#2537=FACE_OUTER_BOUND('',#3933,.T.);
#2538=FACE_OUTER_BOUND('',#3934,.T.);
#2539=FACE_OUTER_BOUND('',#3935,.T.);
#2540=FACE_OUTER_BOUND('',#3936,.T.);
#2541=FACE_OUTER_BOUND('',#3937,.T.);
#2542=FACE_OUTER_BOUND('',#3938,.T.);
#2543=FACE_OUTER_BOUND('',#3939,.T.);
#2544=FACE_OUTER_BOUND('',#3940,.T.);
#2545=FACE_OUTER_BOUND('',#3941,.T.);
#2546=FACE_OUTER_BOUND('',#3942,.T.);
#2547=FACE_OUTER_BOUND('',#3943,.T.);
#2548=FACE_OUTER_BOUND('',#3944,.T.);
#2549=FACE_OUTER_BOUND('',#3945,.T.);
#2550=FACE_OUTER_BOUND('',#3946,.T.);
#2551=FACE_OUTER_BOUND('',#3947,.T.);
#2552=FACE_OUTER_BOUND('',#3948,.T.);
#2553=FACE_OUTER_BOUND('',#3949,.T.);
#2554=FACE_OUTER_BOUND('',#3950,.T.);
#2555=FACE_OUTER_BOUND('',#3951,.T.);
#2556=FACE_OUTER_BOUND('',#3952,.T.);
#2557=FACE_OUTER_BOUND('',#3953,.T.);
#2558=FACE_OUTER_BOUND('',#3954,.T.);
#2559=FACE_OUTER_BOUND('',#3955,.T.);
#2560=FACE_OUTER_BOUND('',#3956,.T.);
#2561=FACE_OUTER_BOUND('',#3957,.T.);
#2562=FACE_OUTER_BOUND('',#3958,.T.);
#2563=FACE_OUTER_BOUND('',#3959,.T.);
#2564=FACE_OUTER_BOUND('',#3960,.T.);
#2565=FACE_OUTER_BOUND('',#3961,.T.);
#2566=FACE_OUTER_BOUND('',#3962,.T.);
#2567=FACE_OUTER_BOUND('',#3963,.T.);
#2568=FACE_OUTER_BOUND('',#3964,.T.);
#2569=FACE_OUTER_BOUND('',#3965,.T.);
#2570=FACE_OUTER_BOUND('',#3966,.T.);
#2571=FACE_OUTER_BOUND('',#3967,.T.);
#2572=FACE_OUTER_BOUND('',#3968,.T.);
#2573=FACE_OUTER_BOUND('',#3969,.T.);
#2574=FACE_OUTER_BOUND('',#3970,.T.);
#2575=FACE_OUTER_BOUND('',#3971,.T.);
#2576=FACE_OUTER_BOUND('',#3972,.T.);
#2577=FACE_OUTER_BOUND('',#3973,.T.);
#2578=FACE_OUTER_BOUND('',#3974,.T.);
#2579=FACE_OUTER_BOUND('',#3975,.T.);
#2580=FACE_OUTER_BOUND('',#3976,.T.);
#2581=FACE_OUTER_BOUND('',#3977,.T.);
#2582=FACE_OUTER_BOUND('',#3978,.T.);
#2583=FACE_OUTER_BOUND('',#3979,.T.);
#2584=FACE_OUTER_BOUND('',#3980,.T.);
#2585=FACE_OUTER_BOUND('',#3981,.T.);
#2586=FACE_OUTER_BOUND('',#3982,.T.);
#2587=FACE_OUTER_BOUND('',#3983,.T.);
#2588=FACE_OUTER_BOUND('',#3984,.T.);
#2589=FACE_OUTER_BOUND('',#3985,.T.);
#2590=FACE_OUTER_BOUND('',#3986,.T.);
#2591=FACE_OUTER_BOUND('',#3987,.T.);
#2592=FACE_OUTER_BOUND('',#3988,.T.);
#2593=FACE_OUTER_BOUND('',#3989,.T.);
#2594=FACE_OUTER_BOUND('',#3990,.T.);
#2595=FACE_OUTER_BOUND('',#3991,.T.);
#2596=FACE_OUTER_BOUND('',#3992,.T.);
#2597=FACE_OUTER_BOUND('',#3993,.T.);
#2598=FACE_OUTER_BOUND('',#3994,.T.);
#2599=FACE_OUTER_BOUND('',#3995,.T.);
#2600=FACE_OUTER_BOUND('',#3996,.T.);
#2601=FACE_OUTER_BOUND('',#3997,.T.);
#2602=FACE_OUTER_BOUND('',#3998,.T.);
#2603=FACE_OUTER_BOUND('',#3999,.T.);
#2604=FACE_OUTER_BOUND('',#4000,.T.);
#2605=FACE_OUTER_BOUND('',#4001,.T.);
#2606=FACE_OUTER_BOUND('',#4002,.T.);
#2607=FACE_OUTER_BOUND('',#4003,.T.);
#2608=FACE_OUTER_BOUND('',#4004,.T.);
#2609=FACE_OUTER_BOUND('',#4005,.T.);
#2610=FACE_OUTER_BOUND('',#4006,.T.);
#2611=FACE_OUTER_BOUND('',#4007,.T.);
#2612=FACE_OUTER_BOUND('',#4008,.T.);
#2613=FACE_OUTER_BOUND('',#4009,.T.);
#2614=FACE_OUTER_BOUND('',#4010,.T.);
#2615=FACE_OUTER_BOUND('',#4011,.T.);
#2616=FACE_OUTER_BOUND('',#4012,.T.);
#2617=FACE_OUTER_BOUND('',#4013,.T.);
#2618=FACE_OUTER_BOUND('',#4014,.T.);
#2619=FACE_OUTER_BOUND('',#4015,.T.);
#2620=FACE_OUTER_BOUND('',#4016,.T.);
#2621=FACE_OUTER_BOUND('',#4017,.T.);
#2622=FACE_OUTER_BOUND('',#4018,.T.);
#2623=FACE_OUTER_BOUND('',#4019,.T.);
#2624=FACE_OUTER_BOUND('',#4020,.T.);
#2625=FACE_OUTER_BOUND('',#4021,.T.);
#2626=FACE_OUTER_BOUND('',#4022,.T.);
#2627=FACE_OUTER_BOUND('',#4023,.T.);
#2628=FACE_OUTER_BOUND('',#4024,.T.);
#2629=FACE_OUTER_BOUND('',#4025,.T.);
#2630=FACE_OUTER_BOUND('',#4026,.T.);
#2631=FACE_OUTER_BOUND('',#4027,.T.);
#2632=FACE_OUTER_BOUND('',#4028,.T.);
#2633=FACE_OUTER_BOUND('',#4029,.T.);
#2634=FACE_OUTER_BOUND('',#4030,.T.);
#2635=FACE_OUTER_BOUND('',#4031,.T.);
#2636=FACE_OUTER_BOUND('',#4032,.T.);
#2637=FACE_OUTER_BOUND('',#4033,.T.);
#2638=FACE_OUTER_BOUND('',#4034,.T.);
#2639=FACE_OUTER_BOUND('',#4035,.T.);
#2640=FACE_OUTER_BOUND('',#4036,.T.);
#2641=FACE_OUTER_BOUND('',#4037,.T.);
#2642=FACE_OUTER_BOUND('',#4038,.T.);
#2643=FACE_OUTER_BOUND('',#4039,.T.);
#2644=FACE_OUTER_BOUND('',#4040,.T.);
#2645=FACE_OUTER_BOUND('',#4041,.T.);
#2646=FACE_OUTER_BOUND('',#4042,.T.);
#2647=FACE_OUTER_BOUND('',#4043,.T.);
#2648=FACE_OUTER_BOUND('',#4044,.T.);
#2649=FACE_OUTER_BOUND('',#4045,.T.);
#2650=FACE_OUTER_BOUND('',#4046,.T.);
#2651=FACE_OUTER_BOUND('',#4047,.T.);
#2652=FACE_OUTER_BOUND('',#4048,.T.);
#2653=FACE_OUTER_BOUND('',#4049,.T.);
#2654=FACE_OUTER_BOUND('',#4050,.T.);
#2655=FACE_OUTER_BOUND('',#4051,.T.);
#2656=FACE_OUTER_BOUND('',#4052,.T.);
#2657=FACE_OUTER_BOUND('',#4053,.T.);
#2658=FACE_OUTER_BOUND('',#4054,.T.);
#2659=FACE_OUTER_BOUND('',#4055,.T.);
#2660=FACE_OUTER_BOUND('',#4056,.T.);
#2661=FACE_OUTER_BOUND('',#4057,.T.);
#2662=FACE_OUTER_BOUND('',#4058,.T.);
#2663=FACE_OUTER_BOUND('',#4059,.T.);
#2664=FACE_OUTER_BOUND('',#4060,.T.);
#2665=FACE_OUTER_BOUND('',#4061,.T.);
#2666=FACE_OUTER_BOUND('',#4062,.T.);
#2667=FACE_OUTER_BOUND('',#4063,.T.);
#2668=FACE_OUTER_BOUND('',#4064,.T.);
#2669=FACE_OUTER_BOUND('',#4065,.T.);
#2670=FACE_OUTER_BOUND('',#4066,.T.);
#2671=FACE_OUTER_BOUND('',#4067,.T.);
#2672=FACE_OUTER_BOUND('',#4068,.T.);
#2673=FACE_OUTER_BOUND('',#4069,.T.);
#2674=FACE_OUTER_BOUND('',#4070,.T.);
#2675=FACE_OUTER_BOUND('',#4071,.T.);
#2676=FACE_OUTER_BOUND('',#4072,.T.);
#2677=FACE_OUTER_BOUND('',#4073,.T.);
#2678=FACE_OUTER_BOUND('',#4074,.T.);
#2679=FACE_OUTER_BOUND('',#4075,.T.);
#2680=FACE_OUTER_BOUND('',#4076,.T.);
#2681=FACE_OUTER_BOUND('',#4077,.T.);
#2682=FACE_OUTER_BOUND('',#4078,.T.);
#2683=FACE_OUTER_BOUND('',#4079,.T.);
#2684=FACE_OUTER_BOUND('',#4080,.T.);
#2685=FACE_OUTER_BOUND('',#4081,.T.);
#2686=FACE_OUTER_BOUND('',#4082,.T.);
#2687=FACE_OUTER_BOUND('',#4083,.T.);
#2688=FACE_OUTER_BOUND('',#4084,.T.);
#2689=FACE_OUTER_BOUND('',#4085,.T.);
#2690=FACE_OUTER_BOUND('',#4086,.T.);
#2691=FACE_OUTER_BOUND('',#4087,.T.);
#2692=FACE_OUTER_BOUND('',#4088,.T.);
#2693=FACE_OUTER_BOUND('',#4089,.T.);
#2694=FACE_OUTER_BOUND('',#4090,.T.);
#2695=FACE_OUTER_BOUND('',#4091,.T.);
#2696=FACE_OUTER_BOUND('',#4092,.T.);
#2697=FACE_OUTER_BOUND('',#4093,.T.);
#2698=FACE_OUTER_BOUND('',#4094,.T.);
#2699=FACE_OUTER_BOUND('',#4095,.T.);
#2700=FACE_OUTER_BOUND('',#4096,.T.);
#2701=FACE_OUTER_BOUND('',#4097,.T.);
#2702=FACE_OUTER_BOUND('',#4098,.T.);
#2703=FACE_OUTER_BOUND('',#4099,.T.);
#2704=FACE_OUTER_BOUND('',#4100,.T.);
#2705=FACE_OUTER_BOUND('',#4101,.T.);
#2706=FACE_OUTER_BOUND('',#4102,.T.);
#2707=FACE_OUTER_BOUND('',#4103,.T.);
#2708=FACE_OUTER_BOUND('',#4104,.T.);
#2709=FACE_OUTER_BOUND('',#4105,.T.);
#2710=FACE_OUTER_BOUND('',#4106,.T.);
#2711=FACE_OUTER_BOUND('',#4107,.T.);
#2712=FACE_OUTER_BOUND('',#4108,.T.);
#2713=FACE_OUTER_BOUND('',#4109,.T.);
#2714=FACE_OUTER_BOUND('',#4110,.T.);
#2715=FACE_OUTER_BOUND('',#4111,.T.);
#2716=FACE_OUTER_BOUND('',#4112,.T.);
#2717=FACE_OUTER_BOUND('',#4113,.T.);
#2718=FACE_OUTER_BOUND('',#4114,.T.);
#2719=FACE_OUTER_BOUND('',#4115,.T.);
#2720=FACE_OUTER_BOUND('',#4116,.T.);
#2721=FACE_OUTER_BOUND('',#4117,.T.);
#2722=FACE_OUTER_BOUND('',#4118,.T.);
#2723=FACE_OUTER_BOUND('',#4119,.T.);
#2724=FACE_OUTER_BOUND('',#4120,.T.);
#2725=FACE_OUTER_BOUND('',#4121,.T.);
#2726=FACE_OUTER_BOUND('',#4122,.T.);
#2727=FACE_OUTER_BOUND('',#4123,.T.);
#2728=FACE_OUTER_BOUND('',#4124,.T.);
#2729=FACE_OUTER_BOUND('',#4125,.T.);
#2730=FACE_OUTER_BOUND('',#4126,.T.);
#2731=FACE_OUTER_BOUND('',#4127,.T.);
#2732=FACE_OUTER_BOUND('',#4128,.T.);
#2733=FACE_OUTER_BOUND('',#4129,.T.);
#2734=FACE_OUTER_BOUND('',#4130,.T.);
#2735=FACE_OUTER_BOUND('',#4131,.T.);
#2736=FACE_OUTER_BOUND('',#4132,.T.);
#2737=FACE_OUTER_BOUND('',#4133,.T.);
#2738=FACE_OUTER_BOUND('',#4134,.T.);
#2739=FACE_OUTER_BOUND('',#4135,.T.);
#2740=FACE_OUTER_BOUND('',#4136,.T.);
#2741=FACE_OUTER_BOUND('',#4137,.T.);
#2742=FACE_OUTER_BOUND('',#4138,.T.);
#2743=FACE_OUTER_BOUND('',#4139,.T.);
#2744=FACE_OUTER_BOUND('',#4140,.T.);
#2745=FACE_OUTER_BOUND('',#4141,.T.);
#2746=FACE_OUTER_BOUND('',#4142,.T.);
#2747=FACE_OUTER_BOUND('',#4143,.T.);
#2748=FACE_OUTER_BOUND('',#4144,.T.);
#2749=FACE_OUTER_BOUND('',#4145,.T.);
#2750=FACE_OUTER_BOUND('',#4146,.T.);
#2751=FACE_OUTER_BOUND('',#4147,.T.);
#2752=FACE_OUTER_BOUND('',#4148,.T.);
#2753=FACE_OUTER_BOUND('',#4149,.T.);
#2754=FACE_OUTER_BOUND('',#4150,.T.);
#2755=FACE_OUTER_BOUND('',#4151,.T.);
#2756=FACE_OUTER_BOUND('',#4152,.T.);
#2757=FACE_OUTER_BOUND('',#4153,.T.);
#2758=FACE_OUTER_BOUND('',#4154,.T.);
#2759=FACE_OUTER_BOUND('',#4159,.T.);
#2760=FACE_OUTER_BOUND('',#4162,.T.);
#2761=FACE_OUTER_BOUND('',#4163,.T.);
#2762=FACE_OUTER_BOUND('',#4165,.T.);
#2763=FACE_OUTER_BOUND('',#4166,.T.);
#2764=FACE_OUTER_BOUND('',#4167,.T.);
#2765=FACE_OUTER_BOUND('',#4169,.T.);
#2766=FACE_OUTER_BOUND('',#4170,.T.);
#2767=FACE_OUTER_BOUND('',#4172,.T.);
#2768=FACE_OUTER_BOUND('',#4173,.T.);
#2769=FACE_OUTER_BOUND('',#4175,.T.);
#2770=FACE_OUTER_BOUND('',#4176,.T.);
#2771=FACE_OUTER_BOUND('',#4177,.T.);
#2772=FACE_OUTER_BOUND('',#4178,.T.);
#2773=FACE_OUTER_BOUND('',#4179,.T.);
#2774=FACE_OUTER_BOUND('',#4180,.T.);
#2775=FACE_OUTER_BOUND('',#4181,.T.);
#2776=FACE_OUTER_BOUND('',#4182,.T.);
#2777=FACE_OUTER_BOUND('',#4183,.T.);
#2778=FACE_OUTER_BOUND('',#4184,.T.);
#2779=FACE_OUTER_BOUND('',#4185,.T.);
#2780=FACE_OUTER_BOUND('',#4188,.T.);
#2781=FACE_OUTER_BOUND('',#4189,.T.);
#2782=FACE_OUTER_BOUND('',#4190,.T.);
#2783=FACE_OUTER_BOUND('',#4191,.T.);
#2784=FACE_OUTER_BOUND('',#4192,.T.);
#2785=FACE_OUTER_BOUND('',#4195,.T.);
#2786=FACE_OUTER_BOUND('',#4196,.T.);
#2787=FACE_OUTER_BOUND('',#4197,.T.);
#2788=FACE_OUTER_BOUND('',#4198,.T.);
#2789=FACE_OUTER_BOUND('',#4199,.T.);
#2790=FACE_OUTER_BOUND('',#4200,.T.);
#2791=FACE_OUTER_BOUND('',#4201,.T.);
#2792=FACE_OUTER_BOUND('',#4202,.T.);
#2793=FACE_OUTER_BOUND('',#4203,.T.);
#2794=FACE_OUTER_BOUND('',#4204,.T.);
#2795=FACE_OUTER_BOUND('',#4205,.T.);
#2796=FACE_OUTER_BOUND('',#4206,.T.);
#2797=FACE_OUTER_BOUND('',#4207,.T.);
#2798=FACE_OUTER_BOUND('',#4208,.T.);
#2799=FACE_OUTER_BOUND('',#4209,.T.);
#2800=FACE_OUTER_BOUND('',#4210,.T.);
#2801=FACE_OUTER_BOUND('',#4211,.T.);
#2802=FACE_OUTER_BOUND('',#4212,.T.);
#2803=FACE_OUTER_BOUND('',#4213,.T.);
#2804=FACE_OUTER_BOUND('',#4214,.T.);
#2805=FACE_OUTER_BOUND('',#4215,.T.);
#2806=FACE_OUTER_BOUND('',#4216,.T.);
#2807=FACE_OUTER_BOUND('',#4217,.T.);
#2808=FACE_OUTER_BOUND('',#4218,.T.);
#2809=FACE_OUTER_BOUND('',#4219,.T.);
#2810=FACE_OUTER_BOUND('',#4220,.T.);
#2811=FACE_OUTER_BOUND('',#4221,.T.);
#2812=FACE_OUTER_BOUND('',#4222,.T.);
#2813=FACE_OUTER_BOUND('',#4223,.T.);
#2814=FACE_OUTER_BOUND('',#4224,.T.);
#2815=FACE_OUTER_BOUND('',#4225,.T.);
#2816=FACE_OUTER_BOUND('',#4226,.T.);
#2817=FACE_OUTER_BOUND('',#4227,.T.);
#2818=FACE_OUTER_BOUND('',#4228,.T.);
#2819=FACE_OUTER_BOUND('',#4229,.T.);
#2820=FACE_OUTER_BOUND('',#4230,.T.);
#2821=FACE_OUTER_BOUND('',#4231,.T.);
#2822=FACE_OUTER_BOUND('',#4232,.T.);
#2823=FACE_OUTER_BOUND('',#4233,.T.);
#2824=FACE_OUTER_BOUND('',#4234,.T.);
#2825=FACE_OUTER_BOUND('',#4235,.T.);
#2826=FACE_OUTER_BOUND('',#4236,.T.);
#2827=FACE_OUTER_BOUND('',#4237,.T.);
#2828=FACE_OUTER_BOUND('',#4238,.T.);
#2829=FACE_OUTER_BOUND('',#4239,.T.);
#2830=FACE_OUTER_BOUND('',#4240,.T.);
#2831=FACE_OUTER_BOUND('',#4241,.T.);
#2832=FACE_OUTER_BOUND('',#4243,.T.);
#2833=FACE_OUTER_BOUND('',#4244,.T.);
#2834=FACE_OUTER_BOUND('',#4245,.T.);
#2835=FACE_OUTER_BOUND('',#4246,.T.);
#2836=FACE_OUTER_BOUND('',#4247,.T.);
#2837=FACE_OUTER_BOUND('',#4248,.T.);
#2838=FACE_OUTER_BOUND('',#4249,.T.);
#2839=FACE_OUTER_BOUND('',#4250,.T.);
#2840=FACE_OUTER_BOUND('',#4251,.T.);
#2841=FACE_OUTER_BOUND('',#4252,.T.);
#2842=FACE_OUTER_BOUND('',#4254,.T.);
#2843=FACE_OUTER_BOUND('',#4255,.T.);
#2844=FACE_OUTER_BOUND('',#4256,.T.);
#2845=FACE_OUTER_BOUND('',#4257,.T.);
#2846=FACE_OUTER_BOUND('',#4258,.T.);
#2847=FACE_OUTER_BOUND('',#4259,.T.);
#2848=FACE_OUTER_BOUND('',#4260,.T.);
#2849=FACE_OUTER_BOUND('',#4261,.T.);
#2850=FACE_OUTER_BOUND('',#4262,.T.);
#2851=FACE_OUTER_BOUND('',#4263,.T.);
#2852=FACE_OUTER_BOUND('',#4264,.T.);
#2853=FACE_OUTER_BOUND('',#4265,.T.);
#2854=FACE_OUTER_BOUND('',#4267,.T.);
#2855=FACE_OUTER_BOUND('',#4268,.T.);
#2856=FACE_OUTER_BOUND('',#4269,.T.);
#2857=FACE_OUTER_BOUND('',#4271,.T.);
#2858=FACE_OUTER_BOUND('',#4273,.T.);
#2859=FACE_OUTER_BOUND('',#4274,.T.);
#2860=FACE_OUTER_BOUND('',#4275,.T.);
#2861=FACE_OUTER_BOUND('',#4277,.T.);
#2862=FACE_OUTER_BOUND('',#4278,.T.);
#2863=FACE_OUTER_BOUND('',#4280,.T.);
#2864=FACE_OUTER_BOUND('',#4281,.T.);
#2865=FACE_OUTER_BOUND('',#4283,.T.);
#2866=FACE_OUTER_BOUND('',#4284,.T.);
#2867=FACE_OUTER_BOUND('',#4286,.T.);
#2868=FACE_OUTER_BOUND('',#4287,.T.);
#2869=FACE_OUTER_BOUND('',#4288,.T.);
#2870=FACE_OUTER_BOUND('',#4289,.T.);
#2871=FACE_OUTER_BOUND('',#4290,.T.);
#2872=FACE_OUTER_BOUND('',#4291,.T.);
#2873=FACE_OUTER_BOUND('',#4292,.T.);
#2874=FACE_OUTER_BOUND('',#4293,.T.);
#2875=FACE_OUTER_BOUND('',#4294,.T.);
#2876=FACE_OUTER_BOUND('',#4295,.T.);
#2877=FACE_OUTER_BOUND('',#4296,.T.);
#2878=FACE_OUTER_BOUND('',#4297,.T.);
#2879=FACE_OUTER_BOUND('',#4298,.T.);
#2880=FACE_OUTER_BOUND('',#4299,.T.);
#2881=FACE_OUTER_BOUND('',#4300,.T.);
#2882=FACE_OUTER_BOUND('',#4301,.T.);
#2883=FACE_OUTER_BOUND('',#4302,.T.);
#2884=FACE_OUTER_BOUND('',#4303,.T.);
#2885=FACE_OUTER_BOUND('',#4304,.T.);
#2886=FACE_OUTER_BOUND('',#4305,.T.);
#2887=FACE_OUTER_BOUND('',#4306,.T.);
#2888=FACE_OUTER_BOUND('',#4307,.T.);
#2889=FACE_OUTER_BOUND('',#4308,.T.);
#2890=FACE_OUTER_BOUND('',#4309,.T.);
#2891=FACE_OUTER_BOUND('',#4310,.T.);
#2892=FACE_OUTER_BOUND('',#4311,.T.);
#2893=FACE_OUTER_BOUND('',#4312,.T.);
#2894=FACE_OUTER_BOUND('',#4313,.T.);
#2895=FACE_OUTER_BOUND('',#4314,.T.);
#2896=FACE_OUTER_BOUND('',#4315,.T.);
#2897=FACE_OUTER_BOUND('',#4316,.T.);
#2898=FACE_OUTER_BOUND('',#4317,.T.);
#2899=FACE_OUTER_BOUND('',#4318,.T.);
#2900=FACE_OUTER_BOUND('',#4319,.T.);
#2901=FACE_OUTER_BOUND('',#4320,.T.);
#2902=FACE_OUTER_BOUND('',#4321,.T.);
#2903=FACE_OUTER_BOUND('',#4322,.T.);
#2904=FACE_OUTER_BOUND('',#4323,.T.);
#2905=FACE_OUTER_BOUND('',#4324,.T.);
#2906=FACE_OUTER_BOUND('',#4325,.T.);
#2907=FACE_OUTER_BOUND('',#4326,.T.);
#2908=FACE_OUTER_BOUND('',#4327,.T.);
#2909=FACE_OUTER_BOUND('',#4328,.T.);
#2910=FACE_OUTER_BOUND('',#4329,.T.);
#2911=FACE_OUTER_BOUND('',#4330,.T.);
#2912=FACE_OUTER_BOUND('',#4331,.T.);
#2913=FACE_OUTER_BOUND('',#4332,.T.);
#2914=FACE_OUTER_BOUND('',#4333,.T.);
#2915=FACE_OUTER_BOUND('',#4334,.T.);
#2916=FACE_OUTER_BOUND('',#4335,.T.);
#2917=FACE_OUTER_BOUND('',#4336,.T.);
#2918=FACE_OUTER_BOUND('',#4337,.T.);
#2919=FACE_OUTER_BOUND('',#4338,.T.);
#2920=FACE_OUTER_BOUND('',#4339,.T.);
#2921=FACE_OUTER_BOUND('',#4340,.T.);
#2922=FACE_OUTER_BOUND('',#4341,.T.);
#2923=FACE_OUTER_BOUND('',#4342,.T.);
#2924=FACE_OUTER_BOUND('',#4343,.T.);
#2925=FACE_OUTER_BOUND('',#4344,.T.);
#2926=FACE_OUTER_BOUND('',#4345,.T.);
#2927=FACE_OUTER_BOUND('',#4346,.T.);
#2928=FACE_OUTER_BOUND('',#4347,.T.);
#2929=FACE_OUTER_BOUND('',#4348,.T.);
#2930=FACE_OUTER_BOUND('',#4349,.T.);
#2931=FACE_OUTER_BOUND('',#4350,.T.);
#2932=FACE_OUTER_BOUND('',#4351,.T.);
#2933=FACE_OUTER_BOUND('',#4352,.T.);
#2934=FACE_OUTER_BOUND('',#4353,.T.);
#2935=FACE_OUTER_BOUND('',#4354,.T.);
#2936=FACE_OUTER_BOUND('',#4355,.T.);
#2937=FACE_OUTER_BOUND('',#4356,.T.);
#2938=FACE_OUTER_BOUND('',#4357,.T.);
#2939=FACE_OUTER_BOUND('',#4358,.T.);
#2940=FACE_OUTER_BOUND('',#4359,.T.);
#2941=FACE_OUTER_BOUND('',#4360,.T.);
#2942=FACE_OUTER_BOUND('',#4361,.T.);
#2943=FACE_OUTER_BOUND('',#4362,.T.);
#2944=FACE_OUTER_BOUND('',#4363,.T.);
#2945=FACE_OUTER_BOUND('',#4364,.T.);
#2946=FACE_OUTER_BOUND('',#4365,.T.);
#2947=FACE_OUTER_BOUND('',#4366,.T.);
#2948=FACE_OUTER_BOUND('',#4367,.T.);
#2949=FACE_OUTER_BOUND('',#4368,.T.);
#2950=FACE_OUTER_BOUND('',#4369,.T.);
#2951=FACE_OUTER_BOUND('',#4370,.T.);
#2952=FACE_OUTER_BOUND('',#4371,.T.);
#2953=FACE_OUTER_BOUND('',#4372,.T.);
#2954=FACE_OUTER_BOUND('',#4373,.T.);
#2955=FACE_OUTER_BOUND('',#4374,.T.);
#2956=FACE_OUTER_BOUND('',#4375,.T.);
#2957=FACE_OUTER_BOUND('',#4376,.T.);
#2958=FACE_OUTER_BOUND('',#4377,.T.);
#2959=FACE_OUTER_BOUND('',#4378,.T.);
#2960=FACE_OUTER_BOUND('',#4379,.T.);
#2961=FACE_OUTER_BOUND('',#4380,.T.);
#2962=FACE_OUTER_BOUND('',#4381,.T.);
#2963=FACE_OUTER_BOUND('',#4382,.T.);
#2964=FACE_OUTER_BOUND('',#4383,.T.);
#2965=FACE_OUTER_BOUND('',#4384,.T.);
#2966=FACE_OUTER_BOUND('',#4385,.T.);
#2967=FACE_OUTER_BOUND('',#4386,.T.);
#2968=FACE_OUTER_BOUND('',#4387,.T.);
#2969=FACE_OUTER_BOUND('',#4388,.T.);
#2970=FACE_OUTER_BOUND('',#4389,.T.);
#2971=FACE_OUTER_BOUND('',#4390,.T.);
#2972=FACE_OUTER_BOUND('',#4391,.T.);
#2973=FACE_OUTER_BOUND('',#4392,.T.);
#2974=FACE_OUTER_BOUND('',#4393,.T.);
#2975=FACE_OUTER_BOUND('',#4394,.T.);
#2976=FACE_OUTER_BOUND('',#4395,.T.);
#2977=FACE_OUTER_BOUND('',#4396,.T.);
#2978=FACE_OUTER_BOUND('',#4397,.T.);
#2979=FACE_OUTER_BOUND('',#4398,.T.);
#2980=FACE_OUTER_BOUND('',#4399,.T.);
#2981=FACE_OUTER_BOUND('',#4400,.T.);
#2982=FACE_OUTER_BOUND('',#4401,.T.);
#2983=FACE_OUTER_BOUND('',#4402,.T.);
#2984=FACE_OUTER_BOUND('',#4403,.T.);
#2985=FACE_OUTER_BOUND('',#4404,.T.);
#2986=FACE_OUTER_BOUND('',#4405,.T.);
#2987=FACE_OUTER_BOUND('',#4406,.T.);
#2988=FACE_OUTER_BOUND('',#4407,.T.);
#2989=FACE_OUTER_BOUND('',#4408,.T.);
#2990=FACE_OUTER_BOUND('',#4409,.T.);
#2991=FACE_OUTER_BOUND('',#4410,.T.);
#2992=FACE_OUTER_BOUND('',#4411,.T.);
#2993=FACE_OUTER_BOUND('',#4412,.T.);
#2994=FACE_OUTER_BOUND('',#4413,.T.);
#2995=FACE_OUTER_BOUND('',#4414,.T.);
#2996=FACE_OUTER_BOUND('',#4415,.T.);
#2997=FACE_OUTER_BOUND('',#4416,.T.);
#2998=FACE_OUTER_BOUND('',#4417,.T.);
#2999=FACE_OUTER_BOUND('',#4418,.T.);
#3000=FACE_OUTER_BOUND('',#4419,.T.);
#3001=FACE_OUTER_BOUND('',#4420,.T.);
#3002=FACE_OUTER_BOUND('',#4421,.T.);
#3003=FACE_OUTER_BOUND('',#4422,.T.);
#3004=FACE_OUTER_BOUND('',#4423,.T.);
#3005=FACE_OUTER_BOUND('',#4424,.T.);
#3006=FACE_OUTER_BOUND('',#4425,.T.);
#3007=FACE_OUTER_BOUND('',#4426,.T.);
#3008=FACE_OUTER_BOUND('',#4427,.T.);
#3009=FACE_OUTER_BOUND('',#4428,.T.);
#3010=FACE_OUTER_BOUND('',#4429,.T.);
#3011=FACE_OUTER_BOUND('',#4430,.T.);
#3012=FACE_OUTER_BOUND('',#4431,.T.);
#3013=FACE_OUTER_BOUND('',#4432,.T.);
#3014=FACE_OUTER_BOUND('',#4433,.T.);
#3015=FACE_OUTER_BOUND('',#4434,.T.);
#3016=FACE_OUTER_BOUND('',#4435,.T.);
#3017=FACE_OUTER_BOUND('',#4436,.T.);
#3018=FACE_OUTER_BOUND('',#4437,.T.);
#3019=FACE_OUTER_BOUND('',#4438,.T.);
#3020=FACE_OUTER_BOUND('',#4439,.T.);
#3021=FACE_OUTER_BOUND('',#4440,.T.);
#3022=FACE_OUTER_BOUND('',#4441,.T.);
#3023=FACE_OUTER_BOUND('',#4442,.T.);
#3024=FACE_OUTER_BOUND('',#4443,.T.);
#3025=FACE_OUTER_BOUND('',#4444,.T.);
#3026=FACE_OUTER_BOUND('',#4445,.T.);
#3027=FACE_OUTER_BOUND('',#4446,.T.);
#3028=FACE_OUTER_BOUND('',#4447,.T.);
#3029=FACE_OUTER_BOUND('',#4448,.T.);
#3030=FACE_OUTER_BOUND('',#4449,.T.);
#3031=FACE_OUTER_BOUND('',#4450,.T.);
#3032=FACE_OUTER_BOUND('',#4451,.T.);
#3033=FACE_OUTER_BOUND('',#4452,.T.);
#3034=FACE_OUTER_BOUND('',#4453,.T.);
#3035=FACE_OUTER_BOUND('',#4454,.T.);
#3036=FACE_OUTER_BOUND('',#4455,.T.);
#3037=FACE_OUTER_BOUND('',#4456,.T.);
#3038=FACE_OUTER_BOUND('',#4457,.T.);
#3039=FACE_OUTER_BOUND('',#4458,.T.);
#3040=FACE_OUTER_BOUND('',#4459,.T.);
#3041=FACE_OUTER_BOUND('',#4460,.T.);
#3042=FACE_OUTER_BOUND('',#4461,.T.);
#3043=FACE_OUTER_BOUND('',#4462,.T.);
#3044=FACE_OUTER_BOUND('',#4463,.T.);
#3045=FACE_OUTER_BOUND('',#4464,.T.);
#3046=FACE_OUTER_BOUND('',#4465,.T.);
#3047=FACE_OUTER_BOUND('',#4466,.T.);
#3048=FACE_OUTER_BOUND('',#4467,.T.);
#3049=FACE_OUTER_BOUND('',#4468,.T.);
#3050=FACE_OUTER_BOUND('',#4469,.T.);
#3051=FACE_OUTER_BOUND('',#4470,.T.);
#3052=FACE_OUTER_BOUND('',#4471,.T.);
#3053=FACE_OUTER_BOUND('',#4472,.T.);
#3054=FACE_OUTER_BOUND('',#4473,.T.);
#3055=FACE_OUTER_BOUND('',#4474,.T.);
#3056=FACE_OUTER_BOUND('',#4475,.T.);
#3057=FACE_OUTER_BOUND('',#4476,.T.);
#3058=FACE_OUTER_BOUND('',#4477,.T.);
#3059=FACE_OUTER_BOUND('',#4478,.T.);
#3060=FACE_OUTER_BOUND('',#4479,.T.);
#3061=FACE_OUTER_BOUND('',#4480,.T.);
#3062=FACE_OUTER_BOUND('',#4481,.T.);
#3063=FACE_OUTER_BOUND('',#4482,.T.);
#3064=FACE_OUTER_BOUND('',#4483,.T.);
#3065=FACE_OUTER_BOUND('',#4484,.T.);
#3066=FACE_OUTER_BOUND('',#4485,.T.);
#3067=FACE_OUTER_BOUND('',#4486,.T.);
#3068=FACE_OUTER_BOUND('',#4487,.T.);
#3069=FACE_OUTER_BOUND('',#4488,.T.);
#3070=FACE_OUTER_BOUND('',#4490,.T.);
#3071=FACE_OUTER_BOUND('',#4526,.T.);
#3072=FACE_OUTER_BOUND('',#4527,.T.);
#3073=FACE_OUTER_BOUND('',#4529,.T.);
#3074=FACE_OUTER_BOUND('',#4530,.T.);
#3075=FACE_OUTER_BOUND('',#4531,.T.);
#3076=FACE_OUTER_BOUND('',#4532,.T.);
#3077=FACE_OUTER_BOUND('',#4533,.T.);
#3078=EDGE_LOOP('',(#16528,#16529,#16530,#16531));
#3079=EDGE_LOOP('',(#16532));
#3080=EDGE_LOOP('',(#16533));
#3081=EDGE_LOOP('',(#16534,#16535,#16536,#16537));
#3082=EDGE_LOOP('',(#16538,#16539,#16540,#16541));
#3083=EDGE_LOOP('',(#16542));
#3084=EDGE_LOOP('',(#16543));
#3085=EDGE_LOOP('',(#16544,#16545,#16546,#16547));
#3086=EDGE_LOOP('',(#16548,#16549,#16550,#16551,#16552));
#3087=EDGE_LOOP('',(#16553,#16554,#16555,#16556,#16557));
#3088=EDGE_LOOP('',(#16558));
#3089=EDGE_LOOP('',(#16559));
#3090=EDGE_LOOP('',(#16560,#16561,#16562,#16563));
#3091=EDGE_LOOP('',(#16564,#16565,#16566,#16567));
#3092=EDGE_LOOP('',(#16568));
#3093=EDGE_LOOP('',(#16569,#16570,#16571,#16572));
#3094=EDGE_LOOP('',(#16573,#16574,#16575,#16576));
#3095=EDGE_LOOP('',(#16577,#16578,#16579,#16580));
#3096=EDGE_LOOP('',(#16581,#16582,#16583,#16584,#16585,#16586,#16587,#16588,
#16589,#16590));
#3097=EDGE_LOOP('',(#16591));
#3098=EDGE_LOOP('',(#16592,#16593,#16594,#16595,#16596,#16597,#16598,#16599,
#16600,#16601,#16602,#16603,#16604,#16605,#16606,#16607,#16608,#16609,#16610,
#16611,#16612,#16613,#16614,#16615));
#3099=EDGE_LOOP('',(#16616,#16617,#16618,#16619,#16620));
#3100=EDGE_LOOP('',(#16621,#16622,#16623,#16624,#16625));
#3101=EDGE_LOOP('',(#16626,#16627,#16628,#16629,#16630));
#3102=EDGE_LOOP('',(#16631));
#3103=EDGE_LOOP('',(#16632,#16633,#16634,#16635,#16636,#16637));
#3104=EDGE_LOOP('',(#16638,#16639,#16640,#16641));
#3105=EDGE_LOOP('',(#16642,#16643,#16644,#16645));
#3106=EDGE_LOOP('',(#16646,#16647,#16648,#16649));
#3107=EDGE_LOOP('',(#16650,#16651,#16652,#16653));
#3108=EDGE_LOOP('',(#16654,#16655,#16656,#16657,#16658));
#3109=EDGE_LOOP('',(#16659,#16660,#16661,#16662));
#3110=EDGE_LOOP('',(#16663,#16664,#16665,#16666));
#3111=EDGE_LOOP('',(#16667,#16668,#16669,#16670));
#3112=EDGE_LOOP('',(#16671,#16672,#16673,#16674));
#3113=EDGE_LOOP('',(#16675,#16676,#16677,#16678));
#3114=EDGE_LOOP('',(#16679,#16680,#16681,#16682));
#3115=EDGE_LOOP('',(#16683,#16684,#16685,#16686,#16687,#16688,#16689,#16690,
#16691,#16692));
#3116=EDGE_LOOP('',(#16693,#16694,#16695,#16696));
#3117=EDGE_LOOP('',(#16697,#16698,#16699,#16700,#16701,#16702,#16703,#16704,
#16705,#16706));
#3118=EDGE_LOOP('',(#16707,#16708,#16709,#16710));
#3119=EDGE_LOOP('',(#16711,#16712,#16713,#16714));
#3120=EDGE_LOOP('',(#16715,#16716,#16717,#16718));
#3121=EDGE_LOOP('',(#16719,#16720,#16721,#16722,#16723,#16724,#16725,#16726));
#3122=EDGE_LOOP('',(#16727));
#3123=EDGE_LOOP('',(#16728));
#3124=EDGE_LOOP('',(#16729));
#3125=EDGE_LOOP('',(#16730,#16731,#16732,#16733));
#3126=EDGE_LOOP('',(#16734));
#3127=EDGE_LOOP('',(#16735));
#3128=EDGE_LOOP('',(#16736));
#3129=EDGE_LOOP('',(#16737));
#3130=EDGE_LOOP('',(#16738));
#3131=EDGE_LOOP('',(#16739,#16740,#16741,#16742));
#3132=EDGE_LOOP('',(#16743,#16744,#16745,#16746));
#3133=EDGE_LOOP('',(#16747,#16748,#16749,#16750));
#3134=EDGE_LOOP('',(#16751,#16752,#16753,#16754));
#3135=EDGE_LOOP('',(#16755,#16756,#16757,#16758));
#3136=EDGE_LOOP('',(#16759,#16760,#16761,#16762));
#3137=EDGE_LOOP('',(#16763,#16764,#16765,#16766));
#3138=EDGE_LOOP('',(#16767,#16768,#16769,#16770));
#3139=EDGE_LOOP('',(#16771,#16772,#16773,#16774));
#3140=EDGE_LOOP('',(#16775,#16776,#16777,#16778));
#3141=EDGE_LOOP('',(#16779,#16780,#16781,#16782,#16783,#16784));
#3142=EDGE_LOOP('',(#16785,#16786,#16787,#16788));
#3143=EDGE_LOOP('',(#16789,#16790,#16791,#16792));
#3144=EDGE_LOOP('',(#16793,#16794,#16795,#16796));
#3145=EDGE_LOOP('',(#16797,#16798,#16799,#16800));
#3146=EDGE_LOOP('',(#16801,#16802,#16803,#16804,#16805));
#3147=EDGE_LOOP('',(#16806,#16807,#16808,#16809));
#3148=EDGE_LOOP('',(#16810,#16811,#16812,#16813));
#3149=EDGE_LOOP('',(#16814,#16815,#16816,#16817));
#3150=EDGE_LOOP('',(#16818,#16819,#16820,#16821));
#3151=EDGE_LOOP('',(#16822,#16823,#16824,#16825));
#3152=EDGE_LOOP('',(#16826,#16827,#16828,#16829));
#3153=EDGE_LOOP('',(#16830,#16831,#16832,#16833));
#3154=EDGE_LOOP('',(#16834,#16835,#16836,#16837));
#3155=EDGE_LOOP('',(#16838,#16839,#16840,#16841,#16842,#16843));
#3156=EDGE_LOOP('',(#16844,#16845,#16846,#16847));
#3157=EDGE_LOOP('',(#16848,#16849,#16850,#16851));
#3158=EDGE_LOOP('',(#16852,#16853,#16854,#16855));
#3159=EDGE_LOOP('',(#16856,#16857,#16858,#16859));
#3160=EDGE_LOOP('',(#16860,#16861,#16862,#16863));
#3161=EDGE_LOOP('',(#16864,#16865,#16866,#16867));
#3162=EDGE_LOOP('',(#16868,#16869,#16870,#16871));
#3163=EDGE_LOOP('',(#16872,#16873,#16874,#16875));
#3164=EDGE_LOOP('',(#16876,#16877,#16878,#16879));
#3165=EDGE_LOOP('',(#16880,#16881,#16882,#16883));
#3166=EDGE_LOOP('',(#16884,#16885,#16886,#16887));
#3167=EDGE_LOOP('',(#16888,#16889,#16890,#16891));
#3168=EDGE_LOOP('',(#16892,#16893,#16894,#16895));
#3169=EDGE_LOOP('',(#16896,#16897,#16898,#16899));
#3170=EDGE_LOOP('',(#16900,#16901,#16902,#16903));
#3171=EDGE_LOOP('',(#16904,#16905,#16906,#16907));
#3172=EDGE_LOOP('',(#16908,#16909,#16910,#16911));
#3173=EDGE_LOOP('',(#16912,#16913,#16914,#16915));
#3174=EDGE_LOOP('',(#16916,#16917,#16918,#16919));
#3175=EDGE_LOOP('',(#16920,#16921,#16922,#16923));
#3176=EDGE_LOOP('',(#16924,#16925,#16926,#16927));
#3177=EDGE_LOOP('',(#16928,#16929,#16930,#16931));
#3178=EDGE_LOOP('',(#16932,#16933,#16934,#16935));
#3179=EDGE_LOOP('',(#16936,#16937,#16938,#16939));
#3180=EDGE_LOOP('',(#16940,#16941,#16942,#16943));
#3181=EDGE_LOOP('',(#16944,#16945,#16946,#16947));
#3182=EDGE_LOOP('',(#16948,#16949,#16950,#16951));
#3183=EDGE_LOOP('',(#16952,#16953,#16954,#16955));
#3184=EDGE_LOOP('',(#16956,#16957,#16958,#16959));
#3185=EDGE_LOOP('',(#16960,#16961,#16962,#16963));
#3186=EDGE_LOOP('',(#16964,#16965,#16966,#16967));
#3187=EDGE_LOOP('',(#16968,#16969,#16970,#16971));
#3188=EDGE_LOOP('',(#16972,#16973,#16974,#16975));
#3189=EDGE_LOOP('',(#16976,#16977,#16978,#16979));
#3190=EDGE_LOOP('',(#16980,#16981,#16982,#16983));
#3191=EDGE_LOOP('',(#16984,#16985,#16986,#16987));
#3192=EDGE_LOOP('',(#16988,#16989,#16990,#16991));
#3193=EDGE_LOOP('',(#16992,#16993,#16994,#16995));
#3194=EDGE_LOOP('',(#16996,#16997,#16998,#16999));
#3195=EDGE_LOOP('',(#17000,#17001,#17002,#17003));
#3196=EDGE_LOOP('',(#17004,#17005,#17006,#17007));
#3197=EDGE_LOOP('',(#17008,#17009,#17010,#17011));
#3198=EDGE_LOOP('',(#17012,#17013,#17014,#17015));
#3199=EDGE_LOOP('',(#17016,#17017,#17018,#17019));
#3200=EDGE_LOOP('',(#17020,#17021,#17022,#17023));
#3201=EDGE_LOOP('',(#17024,#17025,#17026,#17027));
#3202=EDGE_LOOP('',(#17028,#17029,#17030,#17031));
#3203=EDGE_LOOP('',(#17032,#17033,#17034,#17035));
#3204=EDGE_LOOP('',(#17036,#17037,#17038,#17039));
#3205=EDGE_LOOP('',(#17040,#17041,#17042,#17043));
#3206=EDGE_LOOP('',(#17044,#17045,#17046,#17047));
#3207=EDGE_LOOP('',(#17048,#17049,#17050,#17051));
#3208=EDGE_LOOP('',(#17052,#17053,#17054,#17055));
#3209=EDGE_LOOP('',(#17056,#17057,#17058,#17059));
#3210=EDGE_LOOP('',(#17060,#17061,#17062,#17063));
#3211=EDGE_LOOP('',(#17064,#17065,#17066,#17067));
#3212=EDGE_LOOP('',(#17068,#17069,#17070,#17071,#17072));
#3213=EDGE_LOOP('',(#17073,#17074,#17075,#17076));
#3214=EDGE_LOOP('',(#17077,#17078,#17079,#17080));
#3215=EDGE_LOOP('',(#17081,#17082,#17083,#17084));
#3216=EDGE_LOOP('',(#17085,#17086,#17087,#17088));
#3217=EDGE_LOOP('',(#17089,#17090,#17091,#17092));
#3218=EDGE_LOOP('',(#17093,#17094,#17095,#17096));
#3219=EDGE_LOOP('',(#17097,#17098,#17099,#17100));
#3220=EDGE_LOOP('',(#17101,#17102,#17103,#17104));
#3221=EDGE_LOOP('',(#17105,#17106,#17107,#17108));
#3222=EDGE_LOOP('',(#17109,#17110,#17111,#17112));
#3223=EDGE_LOOP('',(#17113,#17114,#17115,#17116));
#3224=EDGE_LOOP('',(#17117,#17118,#17119,#17120));
#3225=EDGE_LOOP('',(#17121,#17122,#17123,#17124));
#3226=EDGE_LOOP('',(#17125,#17126,#17127,#17128,#17129,#17130,#17131,#17132,
#17133,#17134,#17135,#17136,#17137,#17138,#17139,#17140));
#3227=EDGE_LOOP('',(#17141));
#3228=EDGE_LOOP('',(#17142));
#3229=EDGE_LOOP('',(#17143,#17144,#17145,#17146,#17147));
#3230=EDGE_LOOP('',(#17148,#17149,#17150,#17151));
#3231=EDGE_LOOP('',(#17152,#17153,#17154,#17155,#17156,#17157));
#3232=EDGE_LOOP('',(#17158,#17159,#17160,#17161,#17162,#17163));
#3233=EDGE_LOOP('',(#17164,#17165,#17166));
#3234=EDGE_LOOP('',(#17167,#17168,#17169,#17170,#17171,#17172,#17173));
#3235=EDGE_LOOP('',(#17174,#17175,#17176,#17177,#17178,#17179));
#3236=EDGE_LOOP('',(#17180,#17181));
#3237=EDGE_LOOP('',(#17182,#17183,#17184,#17185));
#3238=EDGE_LOOP('',(#17186,#17187,#17188,#17189));
#3239=EDGE_LOOP('',(#17190,#17191,#17192,#17193));
#3240=EDGE_LOOP('',(#17194,#17195,#17196,#17197));
#3241=EDGE_LOOP('',(#17198,#17199,#17200,#17201));
#3242=EDGE_LOOP('',(#17202,#17203,#17204,#17205));
#3243=EDGE_LOOP('',(#17206,#17207,#17208,#17209));
#3244=EDGE_LOOP('',(#17210,#17211,#17212,#17213));
#3245=EDGE_LOOP('',(#17214,#17215,#17216,#17217));
#3246=EDGE_LOOP('',(#17218,#17219,#17220,#17221));
#3247=EDGE_LOOP('',(#17222,#17223,#17224,#17225));
#3248=EDGE_LOOP('',(#17226,#17227,#17228,#17229));
#3249=EDGE_LOOP('',(#17230,#17231,#17232,#17233));
#3250=EDGE_LOOP('',(#17234,#17235,#17236,#17237));
#3251=EDGE_LOOP('',(#17238,#17239,#17240,#17241));
#3252=EDGE_LOOP('',(#17242,#17243,#17244,#17245));
#3253=EDGE_LOOP('',(#17246,#17247,#17248,#17249));
#3254=EDGE_LOOP('',(#17250,#17251,#17252,#17253));
#3255=EDGE_LOOP('',(#17254,#17255,#17256,#17257));
#3256=EDGE_LOOP('',(#17258));
#3257=EDGE_LOOP('',(#17259,#17260,#17261,#17262));
#3258=EDGE_LOOP('',(#17263));
#3259=EDGE_LOOP('',(#17264));
#3260=EDGE_LOOP('',(#17265));
#3261=EDGE_LOOP('',(#17266,#17267,#17268,#17269));
#3262=EDGE_LOOP('',(#17270));
#3263=EDGE_LOOP('',(#17271));
#3264=EDGE_LOOP('',(#17272,#17273,#17274,#17275));
#3265=EDGE_LOOP('',(#17276,#17277,#17278,#17279));
#3266=EDGE_LOOP('',(#17280,#17281,#17282,#17283,#17284,#17285,#17286,#17287,
#17288,#17289,#17290,#17291,#17292,#17293,#17294,#17295,#17296,#17297,#17298,
#17299,#17300,#17301,#17302,#17303,#17304,#17305));
#3267=EDGE_LOOP('',(#17306));
#3268=EDGE_LOOP('',(#17307));
#3269=EDGE_LOOP('',(#17308,#17309,#17310,#17311));
#3270=EDGE_LOOP('',(#17312,#17313,#17314,#17315));
#3271=EDGE_LOOP('',(#17316,#17317));
#3272=EDGE_LOOP('',(#17318,#17319,#17320,#17321,#17322,#17323,#17324,#17325,
#17326,#17327));
#3273=EDGE_LOOP('',(#17328,#17329,#17330,#17331));
#3274=EDGE_LOOP('',(#17332,#17333,#17334,#17335));
#3275=EDGE_LOOP('',(#17336,#17337,#17338,#17339,#17340));
#3276=EDGE_LOOP('',(#17341,#17342,#17343,#17344,#17345));
#3277=EDGE_LOOP('',(#17346,#17347,#17348,#17349));
#3278=EDGE_LOOP('',(#17350,#17351,#17352,#17353));
#3279=EDGE_LOOP('',(#17354,#17355,#17356,#17357));
#3280=EDGE_LOOP('',(#17358,#17359,#17360,#17361));
#3281=EDGE_LOOP('',(#17362));
#3282=EDGE_LOOP('',(#17363));
#3283=EDGE_LOOP('',(#17364,#17365,#17366,#17367));
#3284=EDGE_LOOP('',(#17368,#17369,#17370,#17371));
#3285=EDGE_LOOP('',(#17372));
#3286=EDGE_LOOP('',(#17373));
#3287=EDGE_LOOP('',(#17374,#17375,#17376,#17377));
#3288=EDGE_LOOP('',(#17378,#17379,#17380,#17381));
#3289=EDGE_LOOP('',(#17382,#17383,#17384,#17385));
#3290=EDGE_LOOP('',(#17386,#17387,#17388,#17389));
#3291=EDGE_LOOP('',(#17390,#17391,#17392,#17393));
#3292=EDGE_LOOP('',(#17394,#17395,#17396,#17397));
#3293=EDGE_LOOP('',(#17398,#17399,#17400,#17401));
#3294=EDGE_LOOP('',(#17402,#17403,#17404,#17405));
#3295=EDGE_LOOP('',(#17406,#17407,#17408,#17409));
#3296=EDGE_LOOP('',(#17410,#17411,#17412,#17413));
#3297=EDGE_LOOP('',(#17414,#17415,#17416,#17417));
#3298=EDGE_LOOP('',(#17418,#17419,#17420,#17421));
#3299=EDGE_LOOP('',(#17422));
#3300=EDGE_LOOP('',(#17423,#17424,#17425,#17426,#17427,#17428,#17429,#17430));
#3301=EDGE_LOOP('',(#17431));
#3302=EDGE_LOOP('',(#17432));
#3303=EDGE_LOOP('',(#17433,#17434));
#3304=EDGE_LOOP('',(#17435));
#3305=EDGE_LOOP('',(#17436));
#3306=EDGE_LOOP('',(#17437));
#3307=EDGE_LOOP('',(#17438));
#3308=EDGE_LOOP('',(#17439,#17440,#17441,#17442));
#3309=EDGE_LOOP('',(#17443,#17444,#17445,#17446));
#3310=EDGE_LOOP('',(#17447,#17448,#17449,#17450));
#3311=EDGE_LOOP('',(#17451,#17452,#17453,#17454));
#3312=EDGE_LOOP('',(#17455,#17456,#17457,#17458));
#3313=EDGE_LOOP('',(#17459,#17460,#17461,#17462));
#3314=EDGE_LOOP('',(#17463,#17464,#17465,#17466));
#3315=EDGE_LOOP('',(#17467,#17468,#17469,#17470));
#3316=EDGE_LOOP('',(#17471,#17472,#17473,#17474));
#3317=EDGE_LOOP('',(#17475,#17476,#17477,#17478));
#3318=EDGE_LOOP('',(#17479,#17480,#17481,#17482));
#3319=EDGE_LOOP('',(#17483,#17484,#17485,#17486,#17487,#17488,#17489,#17490));
#3320=EDGE_LOOP('',(#17491));
#3321=EDGE_LOOP('',(#17492));
#3322=EDGE_LOOP('',(#17493,#17494));
#3323=EDGE_LOOP('',(#17495));
#3324=EDGE_LOOP('',(#17496));
#3325=EDGE_LOOP('',(#17497));
#3326=EDGE_LOOP('',(#17498));
#3327=EDGE_LOOP('',(#17499,#17500,#17501,#17502));
#3328=EDGE_LOOP('',(#17503));
#3329=EDGE_LOOP('',(#17504,#17505,#17506,#17507));
#3330=EDGE_LOOP('',(#17508));
#3331=EDGE_LOOP('',(#17509,#17510,#17511,#17512));
#3332=EDGE_LOOP('',(#17513));
#3333=EDGE_LOOP('',(#17514,#17515,#17516,#17517));
#3334=EDGE_LOOP('',(#17518));
#3335=EDGE_LOOP('',(#17519,#17520,#17521,#17522));
#3336=EDGE_LOOP('',(#17523,#17524,#17525,#17526));
#3337=EDGE_LOOP('',(#17527,#17528,#17529,#17530));
#3338=EDGE_LOOP('',(#17531,#17532,#17533,#17534));
#3339=EDGE_LOOP('',(#17535,#17536,#17537,#17538,#17539,#17540));
#3340=EDGE_LOOP('',(#17541,#17542,#17543,#17544,#17545,#17546,#17547,#17548,
#17549,#17550));
#3341=EDGE_LOOP('',(#17551));
#3342=EDGE_LOOP('',(#17552));
#3343=EDGE_LOOP('',(#17553,#17554,#17555,#17556));
#3344=EDGE_LOOP('',(#17557,#17558,#17559,#17560,#17561,#17562));
#3345=EDGE_LOOP('',(#17563,#17564,#17565,#17566,#17567,#17568,#17569,#17570));
#3346=EDGE_LOOP('',(#17571));
#3347=EDGE_LOOP('',(#17572));
#3348=EDGE_LOOP('',(#17573,#17574,#17575,#17576));
#3349=EDGE_LOOP('',(#17577,#17578,#17579,#17580));
#3350=EDGE_LOOP('',(#17581));
#3351=EDGE_LOOP('',(#17582,#17583,#17584,#17585));
#3352=EDGE_LOOP('',(#17586));
#3353=EDGE_LOOP('',(#17587));
#3354=EDGE_LOOP('',(#17588,#17589,#17590,#17591));
#3355=EDGE_LOOP('',(#17592,#17593,#17594,#17595));
#3356=EDGE_LOOP('',(#17596,#17597,#17598,#17599));
#3357=EDGE_LOOP('',(#17600,#17601,#17602,#17603));
#3358=EDGE_LOOP('',(#17604,#17605,#17606,#17607));
#3359=EDGE_LOOP('',(#17608,#17609,#17610,#17611));
#3360=EDGE_LOOP('',(#17612,#17613,#17614,#17615));
#3361=EDGE_LOOP('',(#17616,#17617,#17618,#17619,#17620,#17621,#17622,#17623));
#3362=EDGE_LOOP('',(#17624));
#3363=EDGE_LOOP('',(#17625));
#3364=EDGE_LOOP('',(#17626));
#3365=EDGE_LOOP('',(#17627));
#3366=EDGE_LOOP('',(#17628));
#3367=EDGE_LOOP('',(#17629));
#3368=EDGE_LOOP('',(#17630,#17631,#17632,#17633));
#3369=EDGE_LOOP('',(#17634,#17635,#17636,#17637));
#3370=EDGE_LOOP('',(#17638,#17639,#17640,#17641));
#3371=EDGE_LOOP('',(#17642,#17643,#17644,#17645));
#3372=EDGE_LOOP('',(#17646,#17647,#17648,#17649));
#3373=EDGE_LOOP('',(#17650,#17651,#17652,#17653));
#3374=EDGE_LOOP('',(#17654,#17655,#17656,#17657));
#3375=EDGE_LOOP('',(#17658,#17659,#17660,#17661));
#3376=EDGE_LOOP('',(#17662,#17663,#17664,#17665,#17666,#17667));
#3377=EDGE_LOOP('',(#17668,#17669,#17670,#17671,#17672,#17673,#17674,#17675,
#17676,#17677));
#3378=EDGE_LOOP('',(#17678,#17679,#17680,#17681));
#3379=EDGE_LOOP('',(#17682,#17683,#17684,#17685,#17686,#17687));
#3380=EDGE_LOOP('',(#17688,#17689,#17690,#17691));
#3381=EDGE_LOOP('',(#17692,#17693,#17694,#17695,#17696,#17697,#17698));
#3382=EDGE_LOOP('',(#17699,#17700,#17701,#17702,#17703,#17704,#17705,#17706,
#17707,#17708));
#3383=EDGE_LOOP('',(#17709,#17710,#17711,#17712,#17713));
#3384=EDGE_LOOP('',(#17714,#17715,#17716,#17717,#17718,#17719,#17720));
#3385=EDGE_LOOP('',(#17721,#17722,#17723,#17724,#17725));
#3386=EDGE_LOOP('',(#17726,#17727,#17728,#17729));
#3387=EDGE_LOOP('',(#17730,#17731,#17732,#17733));
#3388=EDGE_LOOP('',(#17734,#17735,#17736,#17737));
#3389=EDGE_LOOP('',(#17738,#17739,#17740,#17741));
#3390=EDGE_LOOP('',(#17742,#17743,#17744,#17745));
#3391=EDGE_LOOP('',(#17746,#17747,#17748,#17749));
#3392=EDGE_LOOP('',(#17750,#17751,#17752,#17753));
#3393=EDGE_LOOP('',(#17754,#17755,#17756,#17757));
#3394=EDGE_LOOP('',(#17758,#17759,#17760,#17761));
#3395=EDGE_LOOP('',(#17762,#17763,#17764,#17765));
#3396=EDGE_LOOP('',(#17766,#17767,#17768,#17769));
#3397=EDGE_LOOP('',(#17770,#17771,#17772,#17773));
#3398=EDGE_LOOP('',(#17774,#17775,#17776,#17777));
#3399=EDGE_LOOP('',(#17778,#17779,#17780,#17781));
#3400=EDGE_LOOP('',(#17782,#17783,#17784,#17785));
#3401=EDGE_LOOP('',(#17786,#17787,#17788,#17789));
#3402=EDGE_LOOP('',(#17790,#17791,#17792,#17793));
#3403=EDGE_LOOP('',(#17794,#17795,#17796,#17797));
#3404=EDGE_LOOP('',(#17798,#17799,#17800,#17801));
#3405=EDGE_LOOP('',(#17802,#17803,#17804,#17805));
#3406=EDGE_LOOP('',(#17806,#17807,#17808,#17809));
#3407=EDGE_LOOP('',(#17810,#17811,#17812,#17813));
#3408=EDGE_LOOP('',(#17814,#17815,#17816,#17817));
#3409=EDGE_LOOP('',(#17818,#17819,#17820,#17821));
#3410=EDGE_LOOP('',(#17822,#17823,#17824,#17825));
#3411=EDGE_LOOP('',(#17826,#17827,#17828,#17829));
#3412=EDGE_LOOP('',(#17830,#17831,#17832,#17833,#17834,#17835,#17836,#17837,
#17838,#17839,#17840,#17841,#17842,#17843,#17844,#17845));
#3413=EDGE_LOOP('',(#17846));
#3414=EDGE_LOOP('',(#17847,#17848,#17849,#17850));
#3415=EDGE_LOOP('',(#17851,#17852,#17853,#17854));
#3416=EDGE_LOOP('',(#17855,#17856,#17857,#17858));
#3417=EDGE_LOOP('',(#17859,#17860,#17861,#17862));
#3418=EDGE_LOOP('',(#17863,#17864,#17865,#17866));
#3419=EDGE_LOOP('',(#17867,#17868,#17869,#17870));
#3420=EDGE_LOOP('',(#17871,#17872,#17873,#17874));
#3421=EDGE_LOOP('',(#17875));
#3422=EDGE_LOOP('',(#17876,#17877,#17878,#17879));
#3423=EDGE_LOOP('',(#17880));
#3424=EDGE_LOOP('',(#17881,#17882,#17883,#17884));
#3425=EDGE_LOOP('',(#17885));
#3426=EDGE_LOOP('',(#17886,#17887,#17888,#17889));
#3427=EDGE_LOOP('',(#17890,#17891,#17892,#17893));
#3428=EDGE_LOOP('',(#17894,#17895,#17896,#17897));
#3429=EDGE_LOOP('',(#17898,#17899,#17900,#17901));
#3430=EDGE_LOOP('',(#17902));
#3431=EDGE_LOOP('',(#17903));
#3432=EDGE_LOOP('',(#17904));
#3433=EDGE_LOOP('',(#17905));
#3434=EDGE_LOOP('',(#17906));
#3435=EDGE_LOOP('',(#17907));
#3436=EDGE_LOOP('',(#17908));
#3437=EDGE_LOOP('',(#17909));
#3438=EDGE_LOOP('',(#17910,#17911,#17912,#17913));
#3439=EDGE_LOOP('',(#17914,#17915,#17916,#17917));
#3440=EDGE_LOOP('',(#17918,#17919,#17920,#17921));
#3441=EDGE_LOOP('',(#17922,#17923,#17924,#17925));
#3442=EDGE_LOOP('',(#17926,#17927,#17928,#17929,#17930,#17931));
#3443=EDGE_LOOP('',(#17932,#17933,#17934,#17935,#17936,#17937,#17938,#17939,
#17940,#17941,#17942,#17943,#17944,#17945,#17946,#17947,#17948,#17949,#17950,
#17951,#17952,#17953,#17954,#17955,#17956,#17957,#17958,#17959,#17960,#17961,
#17962,#17963,#17964,#17965,#17966,#17967,#17968,#17969,#17970,#17971,#17972,
#17973,#17974,#17975,#17976,#17977,#17978,#17979,#17980,#17981,#17982,#17983,
#17984,#17985,#17986,#17987,#17988,#17989,#17990,#17991,#17992,#17993,#17994,
#17995,#17996,#17997,#17998,#17999,#18000,#18001,#18002,#18003,#18004,#18005,
#18006,#18007,#18008,#18009,#18010,#18011,#18012,#18013,#18014,#18015,#18016,
#18017,#18018,#18019,#18020,#18021,#18022,#18023,#18024,#18025,#18026,#18027,
#18028,#18029,#18030,#18031,#18032,#18033,#18034,#18035,#18036,#18037,#18038,
#18039,#18040,#18041,#18042,#18043,#18044,#18045,#18046,#18047,#18048,#18049,
#18050,#18051,#18052,#18053,#18054,#18055,#18056,#18057,#18058,#18059,#18060,
#18061,#18062,#18063,#18064,#18065,#18066,#18067,#18068,#18069,#18070,#18071,
#18072,#18073,#18074,#18075,#18076,#18077,#18078,#18079,#18080,#18081,#18082,
#18083,#18084,#18085,#18086,#18087,#18088,#18089,#18090,#18091,#18092,#18093,
#18094,#18095,#18096,#18097,#18098,#18099,#18100,#18101,#18102,#18103,#18104,
#18105,#18106,#18107,#18108,#18109,#18110,#18111,#18112,#18113,#18114,#18115,
#18116,#18117,#18118,#18119,#18120,#18121,#18122,#18123,#18124,#18125,#18126,
#18127,#18128,#18129,#18130,#18131,#18132,#18133,#18134,#18135,#18136,#18137,
#18138,#18139,#18140,#18141,#18142,#18143,#18144,#18145,#18146,#18147,#18148,
#18149,#18150,#18151,#18152,#18153,#18154,#18155,#18156,#18157,#18158,#18159,
#18160,#18161,#18162,#18163,#18164,#18165,#18166,#18167,#18168,#18169,#18170,
#18171));
#3444=EDGE_LOOP('',(#18172));
#3445=EDGE_LOOP('',(#18173,#18174,#18175,#18176,#18177,#18178));
#3446=EDGE_LOOP('',(#18179,#18180,#18181,#18182));
#3447=EDGE_LOOP('',(#18183,#18184,#18185,#18186,#18187,#18188));
#3448=EDGE_LOOP('',(#18189,#18190,#18191,#18192,#18193,#18194));
#3449=EDGE_LOOP('',(#18195,#18196,#18197,#18198));
#3450=EDGE_LOOP('',(#18199,#18200,#18201,#18202,#18203,#18204));
#3451=EDGE_LOOP('',(#18205,#18206,#18207,#18208,#18209,#18210));
#3452=EDGE_LOOP('',(#18211,#18212,#18213,#18214));
#3453=EDGE_LOOP('',(#18215,#18216,#18217,#18218,#18219,#18220));
#3454=EDGE_LOOP('',(#18221,#18222,#18223,#18224,#18225,#18226));
#3455=EDGE_LOOP('',(#18227,#18228,#18229,#18230));
#3456=EDGE_LOOP('',(#18231,#18232,#18233,#18234,#18235,#18236));
#3457=EDGE_LOOP('',(#18237,#18238,#18239,#18240,#18241,#18242));
#3458=EDGE_LOOP('',(#18243,#18244,#18245,#18246));
#3459=EDGE_LOOP('',(#18247,#18248,#18249,#18250,#18251,#18252));
#3460=EDGE_LOOP('',(#18253,#18254,#18255,#18256,#18257,#18258));
#3461=EDGE_LOOP('',(#18259,#18260,#18261,#18262));
#3462=EDGE_LOOP('',(#18263,#18264,#18265,#18266,#18267,#18268));
#3463=EDGE_LOOP('',(#18269,#18270,#18271,#18272,#18273,#18274));
#3464=EDGE_LOOP('',(#18275,#18276,#18277,#18278));
#3465=EDGE_LOOP('',(#18279,#18280,#18281,#18282,#18283,#18284));
#3466=EDGE_LOOP('',(#18285,#18286,#18287,#18288,#18289,#18290));
#3467=EDGE_LOOP('',(#18291,#18292,#18293,#18294));
#3468=EDGE_LOOP('',(#18295,#18296,#18297,#18298,#18299,#18300));
#3469=EDGE_LOOP('',(#18301,#18302,#18303,#18304,#18305,#18306));
#3470=EDGE_LOOP('',(#18307,#18308,#18309,#18310));
#3471=EDGE_LOOP('',(#18311,#18312,#18313,#18314,#18315,#18316));
#3472=EDGE_LOOP('',(#18317,#18318,#18319,#18320,#18321,#18322));
#3473=EDGE_LOOP('',(#18323,#18324,#18325,#18326));
#3474=EDGE_LOOP('',(#18327,#18328,#18329,#18330,#18331,#18332));
#3475=EDGE_LOOP('',(#18333,#18334,#18335,#18336,#18337,#18338));
#3476=EDGE_LOOP('',(#18339,#18340,#18341,#18342));
#3477=EDGE_LOOP('',(#18343,#18344,#18345,#18346,#18347,#18348));
#3478=EDGE_LOOP('',(#18349,#18350,#18351,#18352,#18353,#18354));
#3479=EDGE_LOOP('',(#18355,#18356,#18357,#18358));
#3480=EDGE_LOOP('',(#18359,#18360,#18361,#18362,#18363,#18364));
#3481=EDGE_LOOP('',(#18365,#18366,#18367,#18368));
#3482=EDGE_LOOP('',(#18369,#18370,#18371,#18372));
#3483=EDGE_LOOP('',(#18373,#18374,#18375,#18376,#18377,#18378));
#3484=EDGE_LOOP('',(#18379,#18380,#18381,#18382));
#3485=EDGE_LOOP('',(#18383,#18384,#18385,#18386));
#3486=EDGE_LOOP('',(#18387,#18388,#18389,#18390,#18391,#18392));
#3487=EDGE_LOOP('',(#18393,#18394,#18395,#18396));
#3488=EDGE_LOOP('',(#18397,#18398,#18399,#18400));
#3489=EDGE_LOOP('',(#18401,#18402,#18403,#18404,#18405,#18406));
#3490=EDGE_LOOP('',(#18407,#18408,#18409,#18410));
#3491=EDGE_LOOP('',(#18411,#18412,#18413,#18414));
#3492=EDGE_LOOP('',(#18415,#18416,#18417,#18418,#18419,#18420));
#3493=EDGE_LOOP('',(#18421,#18422,#18423,#18424));
#3494=EDGE_LOOP('',(#18425,#18426,#18427,#18428));
#3495=EDGE_LOOP('',(#18429,#18430,#18431,#18432,#18433,#18434));
#3496=EDGE_LOOP('',(#18435,#18436,#18437,#18438));
#3497=EDGE_LOOP('',(#18439,#18440,#18441,#18442));
#3498=EDGE_LOOP('',(#18443,#18444,#18445,#18446,#18447,#18448));
#3499=EDGE_LOOP('',(#18449,#18450,#18451,#18452));
#3500=EDGE_LOOP('',(#18453,#18454,#18455,#18456));
#3501=EDGE_LOOP('',(#18457,#18458,#18459,#18460,#18461,#18462));
#3502=EDGE_LOOP('',(#18463,#18464,#18465,#18466));
#3503=EDGE_LOOP('',(#18467,#18468,#18469,#18470));
#3504=EDGE_LOOP('',(#18471,#18472,#18473,#18474,#18475,#18476));
#3505=EDGE_LOOP('',(#18477,#18478,#18479,#18480));
#3506=EDGE_LOOP('',(#18481,#18482,#18483,#18484));
#3507=EDGE_LOOP('',(#18485,#18486,#18487,#18488,#18489,#18490));
#3508=EDGE_LOOP('',(#18491,#18492,#18493,#18494));
#3509=EDGE_LOOP('',(#18495,#18496,#18497,#18498));
#3510=EDGE_LOOP('',(#18499,#18500,#18501,#18502,#18503,#18504));
#3511=EDGE_LOOP('',(#18505,#18506,#18507,#18508));
#3512=EDGE_LOOP('',(#18509,#18510,#18511,#18512));
#3513=EDGE_LOOP('',(#18513,#18514,#18515,#18516,#18517,#18518));
#3514=EDGE_LOOP('',(#18519,#18520,#18521,#18522));
#3515=EDGE_LOOP('',(#18523,#18524,#18525,#18526));
#3516=EDGE_LOOP('',(#18527,#18528,#18529,#18530,#18531,#18532));
#3517=EDGE_LOOP('',(#18533,#18534,#18535,#18536,#18537,#18538,#18539,#18540,
#18541,#18542,#18543,#18544,#18545,#18546,#18547,#18548,#18549,#18550,#18551,
#18552,#18553,#18554,#18555,#18556,#18557,#18558,#18559,#18560,#18561,#18562,
#18563,#18564,#18565,#18566,#18567,#18568,#18569,#18570,#18571,#18572,#18573,
#18574,#18575,#18576,#18577,#18578,#18579,#18580,#18581,#18582,#18583,#18584,
#18585,#18586,#18587,#18588,#18589,#18590,#18591,#18592,#18593,#18594,#18595,
#18596,#18597,#18598,#18599,#18600,#18601,#18602,#18603,#18604,#18605,#18606,
#18607,#18608,#18609,#18610,#18611,#18612,#18613,#18614,#18615,#18616,#18617,
#18618,#18619,#18620,#18621,#18622,#18623,#18624,#18625,#18626,#18627,#18628,
#18629,#18630,#18631,#18632,#18633,#18634,#18635,#18636,#18637,#18638,#18639,
#18640,#18641,#18642,#18643,#18644,#18645,#18646,#18647,#18648,#18649,#18650,
#18651,#18652,#18653,#18654,#18655,#18656,#18657,#18658,#18659,#18660,#18661,
#18662,#18663,#18664,#18665,#18666,#18667,#18668,#18669,#18670,#18671,#18672,
#18673,#18674,#18675,#18676,#18677,#18678,#18679,#18680,#18681,#18682,#18683,
#18684,#18685,#18686,#18687,#18688,#18689,#18690,#18691,#18692,#18693,#18694,
#18695,#18696,#18697,#18698,#18699,#18700,#18701,#18702,#18703,#18704,#18705,
#18706,#18707,#18708,#18709,#18710,#18711,#18712,#18713,#18714,#18715,#18716,
#18717,#18718,#18719,#18720,#18721,#18722,#18723,#18724,#18725,#18726,#18727,
#18728,#18729,#18730,#18731,#18732,#18733,#18734,#18735,#18736,#18737,#18738,
#18739,#18740,#18741,#18742,#18743,#18744,#18745,#18746,#18747,#18748,#18749,
#18750,#18751,#18752,#18753,#18754,#18755,#18756,#18757,#18758,#18759,#18760,
#18761,#18762,#18763,#18764,#18765,#18766,#18767,#18768,#18769,#18770,#18771,
#18772));
#3518=EDGE_LOOP('',(#18773));
#3519=EDGE_LOOP('',(#18774,#18775,#18776,#18777,#18778,#18779));
#3520=EDGE_LOOP('',(#18780,#18781,#18782,#18783,#18784,#18785));
#3521=EDGE_LOOP('',(#18786,#18787,#18788,#18789,#18790,#18791));
#3522=EDGE_LOOP('',(#18792,#18793,#18794,#18795,#18796,#18797));
#3523=EDGE_LOOP('',(#18798,#18799,#18800,#18801,#18802,#18803));
#3524=EDGE_LOOP('',(#18804,#18805,#18806,#18807,#18808,#18809));
#3525=EDGE_LOOP('',(#18810,#18811,#18812,#18813,#18814,#18815));
#3526=EDGE_LOOP('',(#18816,#18817,#18818,#18819,#18820,#18821));
#3527=EDGE_LOOP('',(#18822,#18823,#18824,#18825,#18826,#18827));
#3528=EDGE_LOOP('',(#18828,#18829,#18830,#18831,#18832,#18833));
#3529=EDGE_LOOP('',(#18834,#18835,#18836,#18837,#18838,#18839));
#3530=EDGE_LOOP('',(#18840,#18841,#18842,#18843,#18844,#18845));
#3531=EDGE_LOOP('',(#18846,#18847,#18848,#18849,#18850,#18851));
#3532=EDGE_LOOP('',(#18852,#18853,#18854,#18855,#18856,#18857));
#3533=EDGE_LOOP('',(#18858,#18859,#18860,#18861,#18862,#18863));
#3534=EDGE_LOOP('',(#18864,#18865,#18866,#18867,#18868,#18869));
#3535=EDGE_LOOP('',(#18870,#18871,#18872,#18873,#18874,#18875));
#3536=EDGE_LOOP('',(#18876,#18877,#18878,#18879,#18880,#18881));
#3537=EDGE_LOOP('',(#18882,#18883,#18884,#18885,#18886,#18887));
#3538=EDGE_LOOP('',(#18888,#18889,#18890,#18891,#18892,#18893));
#3539=EDGE_LOOP('',(#18894,#18895,#18896,#18897,#18898,#18899));
#3540=EDGE_LOOP('',(#18900,#18901,#18902,#18903,#18904,#18905));
#3541=EDGE_LOOP('',(#18906,#18907,#18908,#18909,#18910,#18911));
#3542=EDGE_LOOP('',(#18912,#18913,#18914,#18915));
#3543=EDGE_LOOP('',(#18916,#18917,#18918,#18919));
#3544=EDGE_LOOP('',(#18920,#18921,#18922,#18923));
#3545=EDGE_LOOP('',(#18924,#18925,#18926,#18927));
#3546=EDGE_LOOP('',(#18928,#18929,#18930,#18931));
#3547=EDGE_LOOP('',(#18932,#18933,#18934,#18935,#18936,#18937));
#3548=EDGE_LOOP('',(#18938,#18939,#18940,#18941));
#3549=EDGE_LOOP('',(#18942,#18943,#18944,#18945));
#3550=EDGE_LOOP('',(#18946,#18947,#18948,#18949));
#3551=EDGE_LOOP('',(#18950,#18951,#18952,#18953));
#3552=EDGE_LOOP('',(#18954,#18955,#18956,#18957));
#3553=EDGE_LOOP('',(#18958,#18959,#18960,#18961));
#3554=EDGE_LOOP('',(#18962,#18963,#18964,#18965));
#3555=EDGE_LOOP('',(#18966,#18967,#18968,#18969));
#3556=EDGE_LOOP('',(#18970,#18971,#18972,#18973));
#3557=EDGE_LOOP('',(#18974,#18975,#18976,#18977));
#3558=EDGE_LOOP('',(#18978,#18979,#18980,#18981));
#3559=EDGE_LOOP('',(#18982,#18983,#18984,#18985));
#3560=EDGE_LOOP('',(#18986,#18987,#18988,#18989));
#3561=EDGE_LOOP('',(#18990,#18991,#18992,#18993));
#3562=EDGE_LOOP('',(#18994,#18995,#18996,#18997));
#3563=EDGE_LOOP('',(#18998,#18999,#19000,#19001));
#3564=EDGE_LOOP('',(#19002,#19003,#19004,#19005,#19006,#19007));
#3565=EDGE_LOOP('',(#19008,#19009,#19010,#19011));
#3566=EDGE_LOOP('',(#19012,#19013,#19014,#19015,#19016,#19017));
#3567=EDGE_LOOP('',(#19018,#19019,#19020,#19021,#19022,#19023));
#3568=EDGE_LOOP('',(#19024,#19025,#19026,#19027));
#3569=EDGE_LOOP('',(#19028,#19029,#19030,#19031));
#3570=EDGE_LOOP('',(#19032,#19033,#19034,#19035));
#3571=EDGE_LOOP('',(#19036,#19037,#19038,#19039));
#3572=EDGE_LOOP('',(#19040,#19041,#19042,#19043));
#3573=EDGE_LOOP('',(#19044,#19045,#19046,#19047));
#3574=EDGE_LOOP('',(#19048,#19049,#19050,#19051));
#3575=EDGE_LOOP('',(#19052,#19053,#19054,#19055));
#3576=EDGE_LOOP('',(#19056,#19057,#19058,#19059));
#3577=EDGE_LOOP('',(#19060,#19061,#19062,#19063));
#3578=EDGE_LOOP('',(#19064,#19065,#19066,#19067));
#3579=EDGE_LOOP('',(#19068,#19069,#19070,#19071));
#3580=EDGE_LOOP('',(#19072,#19073,#19074,#19075));
#3581=EDGE_LOOP('',(#19076,#19077,#19078,#19079));
#3582=EDGE_LOOP('',(#19080,#19081,#19082,#19083));
#3583=EDGE_LOOP('',(#19084,#19085,#19086,#19087));
#3584=EDGE_LOOP('',(#19088,#19089,#19090,#19091,#19092,#19093));
#3585=EDGE_LOOP('',(#19094,#19095,#19096,#19097));
#3586=EDGE_LOOP('',(#19098,#19099,#19100,#19101,#19102,#19103));
#3587=EDGE_LOOP('',(#19104,#19105,#19106,#19107,#19108,#19109));
#3588=EDGE_LOOP('',(#19110,#19111,#19112,#19113));
#3589=EDGE_LOOP('',(#19114,#19115,#19116,#19117));
#3590=EDGE_LOOP('',(#19118,#19119,#19120,#19121));
#3591=EDGE_LOOP('',(#19122,#19123,#19124,#19125));
#3592=EDGE_LOOP('',(#19126,#19127,#19128,#19129));
#3593=EDGE_LOOP('',(#19130,#19131,#19132,#19133));
#3594=EDGE_LOOP('',(#19134,#19135,#19136,#19137));
#3595=EDGE_LOOP('',(#19138,#19139,#19140,#19141));
#3596=EDGE_LOOP('',(#19142,#19143,#19144,#19145));
#3597=EDGE_LOOP('',(#19146,#19147,#19148,#19149));
#3598=EDGE_LOOP('',(#19150,#19151,#19152,#19153));
#3599=EDGE_LOOP('',(#19154,#19155,#19156,#19157));
#3600=EDGE_LOOP('',(#19158,#19159,#19160,#19161));
#3601=EDGE_LOOP('',(#19162,#19163,#19164,#19165));
#3602=EDGE_LOOP('',(#19166,#19167,#19168,#19169));
#3603=EDGE_LOOP('',(#19170,#19171,#19172,#19173));
#3604=EDGE_LOOP('',(#19174,#19175,#19176,#19177,#19178,#19179));
#3605=EDGE_LOOP('',(#19180,#19181,#19182,#19183));
#3606=EDGE_LOOP('',(#19184,#19185,#19186,#19187,#19188,#19189));
#3607=EDGE_LOOP('',(#19190,#19191,#19192,#19193,#19194,#19195));
#3608=EDGE_LOOP('',(#19196,#19197,#19198,#19199));
#3609=EDGE_LOOP('',(#19200,#19201,#19202,#19203));
#3610=EDGE_LOOP('',(#19204,#19205,#19206,#19207));
#3611=EDGE_LOOP('',(#19208,#19209,#19210,#19211));
#3612=EDGE_LOOP('',(#19212,#19213,#19214,#19215));
#3613=EDGE_LOOP('',(#19216,#19217,#19218,#19219));
#3614=EDGE_LOOP('',(#19220,#19221,#19222,#19223));
#3615=EDGE_LOOP('',(#19224,#19225,#19226,#19227));
#3616=EDGE_LOOP('',(#19228,#19229,#19230,#19231));
#3617=EDGE_LOOP('',(#19232,#19233,#19234,#19235));
#3618=EDGE_LOOP('',(#19236,#19237,#19238,#19239));
#3619=EDGE_LOOP('',(#19240,#19241,#19242,#19243));
#3620=EDGE_LOOP('',(#19244,#19245,#19246,#19247));
#3621=EDGE_LOOP('',(#19248,#19249,#19250,#19251));
#3622=EDGE_LOOP('',(#19252,#19253,#19254,#19255));
#3623=EDGE_LOOP('',(#19256,#19257,#19258,#19259));
#3624=EDGE_LOOP('',(#19260,#19261,#19262,#19263,#19264,#19265));
#3625=EDGE_LOOP('',(#19266,#19267,#19268,#19269));
#3626=EDGE_LOOP('',(#19270,#19271,#19272,#19273,#19274,#19275));
#3627=EDGE_LOOP('',(#19276,#19277,#19278,#19279,#19280,#19281));
#3628=EDGE_LOOP('',(#19282,#19283,#19284,#19285));
#3629=EDGE_LOOP('',(#19286,#19287,#19288,#19289));
#3630=EDGE_LOOP('',(#19290,#19291,#19292,#19293));
#3631=EDGE_LOOP('',(#19294,#19295,#19296,#19297));
#3632=EDGE_LOOP('',(#19298,#19299,#19300,#19301));
#3633=EDGE_LOOP('',(#19302,#19303,#19304,#19305));
#3634=EDGE_LOOP('',(#19306,#19307,#19308,#19309));
#3635=EDGE_LOOP('',(#19310,#19311,#19312,#19313));
#3636=EDGE_LOOP('',(#19314,#19315,#19316,#19317));
#3637=EDGE_LOOP('',(#19318,#19319,#19320,#19321));
#3638=EDGE_LOOP('',(#19322,#19323,#19324,#19325));
#3639=EDGE_LOOP('',(#19326,#19327,#19328,#19329));
#3640=EDGE_LOOP('',(#19330,#19331,#19332,#19333));
#3641=EDGE_LOOP('',(#19334,#19335,#19336,#19337));
#3642=EDGE_LOOP('',(#19338,#19339,#19340,#19341));
#3643=EDGE_LOOP('',(#19342,#19343,#19344,#19345));
#3644=EDGE_LOOP('',(#19346,#19347,#19348,#19349,#19350,#19351));
#3645=EDGE_LOOP('',(#19352,#19353,#19354,#19355));
#3646=EDGE_LOOP('',(#19356,#19357,#19358,#19359,#19360,#19361));
#3647=EDGE_LOOP('',(#19362,#19363,#19364,#19365,#19366,#19367));
#3648=EDGE_LOOP('',(#19368,#19369,#19370,#19371));
#3649=EDGE_LOOP('',(#19372,#19373,#19374,#19375));
#3650=EDGE_LOOP('',(#19376,#19377,#19378,#19379));
#3651=EDGE_LOOP('',(#19380,#19381,#19382,#19383));
#3652=EDGE_LOOP('',(#19384,#19385,#19386,#19387));
#3653=EDGE_LOOP('',(#19388,#19389,#19390,#19391));
#3654=EDGE_LOOP('',(#19392,#19393,#19394,#19395));
#3655=EDGE_LOOP('',(#19396,#19397,#19398,#19399));
#3656=EDGE_LOOP('',(#19400,#19401,#19402,#19403));
#3657=EDGE_LOOP('',(#19404,#19405,#19406,#19407));
#3658=EDGE_LOOP('',(#19408,#19409,#19410,#19411));
#3659=EDGE_LOOP('',(#19412,#19413,#19414,#19415));
#3660=EDGE_LOOP('',(#19416,#19417,#19418,#19419));
#3661=EDGE_LOOP('',(#19420,#19421,#19422,#19423));
#3662=EDGE_LOOP('',(#19424,#19425,#19426,#19427));
#3663=EDGE_LOOP('',(#19428,#19429,#19430,#19431));
#3664=EDGE_LOOP('',(#19432,#19433,#19434,#19435,#19436,#19437));
#3665=EDGE_LOOP('',(#19438,#19439,#19440,#19441));
#3666=EDGE_LOOP('',(#19442,#19443,#19444,#19445,#19446,#19447));
#3667=EDGE_LOOP('',(#19448,#19449,#19450,#19451,#19452,#19453));
#3668=EDGE_LOOP('',(#19454,#19455,#19456,#19457));
#3669=EDGE_LOOP('',(#19458,#19459,#19460,#19461));
#3670=EDGE_LOOP('',(#19462,#19463,#19464,#19465));
#3671=EDGE_LOOP('',(#19466,#19467,#19468,#19469));
#3672=EDGE_LOOP('',(#19470,#19471,#19472,#19473));
#3673=EDGE_LOOP('',(#19474,#19475,#19476,#19477));
#3674=EDGE_LOOP('',(#19478,#19479,#19480,#19481));
#3675=EDGE_LOOP('',(#19482,#19483,#19484,#19485));
#3676=EDGE_LOOP('',(#19486,#19487,#19488,#19489));
#3677=EDGE_LOOP('',(#19490,#19491,#19492,#19493));
#3678=EDGE_LOOP('',(#19494,#19495,#19496,#19497));
#3679=EDGE_LOOP('',(#19498,#19499,#19500,#19501));
#3680=EDGE_LOOP('',(#19502,#19503,#19504,#19505));
#3681=EDGE_LOOP('',(#19506,#19507,#19508,#19509));
#3682=EDGE_LOOP('',(#19510,#19511,#19512,#19513));
#3683=EDGE_LOOP('',(#19514,#19515,#19516,#19517));
#3684=EDGE_LOOP('',(#19518,#19519,#19520,#19521,#19522,#19523));
#3685=EDGE_LOOP('',(#19524,#19525,#19526,#19527));
#3686=EDGE_LOOP('',(#19528,#19529,#19530,#19531,#19532,#19533));
#3687=EDGE_LOOP('',(#19534,#19535,#19536,#19537,#19538,#19539));
#3688=EDGE_LOOP('',(#19540,#19541,#19542,#19543));
#3689=EDGE_LOOP('',(#19544,#19545,#19546,#19547));
#3690=EDGE_LOOP('',(#19548,#19549,#19550,#19551));
#3691=EDGE_LOOP('',(#19552,#19553,#19554,#19555));
#3692=EDGE_LOOP('',(#19556,#19557,#19558,#19559));
#3693=EDGE_LOOP('',(#19560,#19561,#19562,#19563));
#3694=EDGE_LOOP('',(#19564,#19565,#19566,#19567));
#3695=EDGE_LOOP('',(#19568,#19569,#19570,#19571));
#3696=EDGE_LOOP('',(#19572,#19573,#19574,#19575));
#3697=EDGE_LOOP('',(#19576,#19577,#19578,#19579));
#3698=EDGE_LOOP('',(#19580,#19581,#19582,#19583));
#3699=EDGE_LOOP('',(#19584,#19585,#19586,#19587));
#3700=EDGE_LOOP('',(#19588,#19589,#19590,#19591));
#3701=EDGE_LOOP('',(#19592,#19593,#19594,#19595));
#3702=EDGE_LOOP('',(#19596,#19597,#19598,#19599));
#3703=EDGE_LOOP('',(#19600,#19601,#19602,#19603));
#3704=EDGE_LOOP('',(#19604,#19605,#19606,#19607,#19608,#19609));
#3705=EDGE_LOOP('',(#19610,#19611,#19612,#19613));
#3706=EDGE_LOOP('',(#19614,#19615,#19616,#19617,#19618,#19619));
#3707=EDGE_LOOP('',(#19620,#19621,#19622,#19623,#19624,#19625));
#3708=EDGE_LOOP('',(#19626,#19627,#19628,#19629));
#3709=EDGE_LOOP('',(#19630,#19631,#19632,#19633));
#3710=EDGE_LOOP('',(#19634,#19635,#19636,#19637));
#3711=EDGE_LOOP('',(#19638,#19639,#19640,#19641));
#3712=EDGE_LOOP('',(#19642,#19643,#19644,#19645));
#3713=EDGE_LOOP('',(#19646,#19647,#19648,#19649));
#3714=EDGE_LOOP('',(#19650,#19651,#19652,#19653));
#3715=EDGE_LOOP('',(#19654,#19655,#19656,#19657));
#3716=EDGE_LOOP('',(#19658,#19659,#19660,#19661));
#3717=EDGE_LOOP('',(#19662,#19663,#19664,#19665));
#3718=EDGE_LOOP('',(#19666,#19667,#19668,#19669));
#3719=EDGE_LOOP('',(#19670,#19671,#19672,#19673));
#3720=EDGE_LOOP('',(#19674,#19675,#19676,#19677));
#3721=EDGE_LOOP('',(#19678,#19679,#19680,#19681));
#3722=EDGE_LOOP('',(#19682,#19683,#19684,#19685));
#3723=EDGE_LOOP('',(#19686,#19687,#19688,#19689));
#3724=EDGE_LOOP('',(#19690,#19691,#19692,#19693,#19694,#19695));
#3725=EDGE_LOOP('',(#19696,#19697,#19698,#19699));
#3726=EDGE_LOOP('',(#19700,#19701,#19702,#19703,#19704,#19705));
#3727=EDGE_LOOP('',(#19706,#19707,#19708,#19709,#19710,#19711));
#3728=EDGE_LOOP('',(#19712,#19713,#19714,#19715));
#3729=EDGE_LOOP('',(#19716,#19717,#19718,#19719));
#3730=EDGE_LOOP('',(#19720,#19721,#19722,#19723));
#3731=EDGE_LOOP('',(#19724,#19725,#19726,#19727));
#3732=EDGE_LOOP('',(#19728,#19729,#19730,#19731));
#3733=EDGE_LOOP('',(#19732,#19733,#19734,#19735));
#3734=EDGE_LOOP('',(#19736,#19737,#19738,#19739));
#3735=EDGE_LOOP('',(#19740,#19741,#19742,#19743));
#3736=EDGE_LOOP('',(#19744,#19745,#19746,#19747));
#3737=EDGE_LOOP('',(#19748,#19749,#19750,#19751));
#3738=EDGE_LOOP('',(#19752,#19753,#19754,#19755));
#3739=EDGE_LOOP('',(#19756,#19757,#19758,#19759));
#3740=EDGE_LOOP('',(#19760,#19761,#19762,#19763));
#3741=EDGE_LOOP('',(#19764,#19765,#19766,#19767));
#3742=EDGE_LOOP('',(#19768,#19769,#19770,#19771));
#3743=EDGE_LOOP('',(#19772,#19773,#19774,#19775));
#3744=EDGE_LOOP('',(#19776,#19777,#19778,#19779,#19780,#19781));
#3745=EDGE_LOOP('',(#19782,#19783,#19784,#19785));
#3746=EDGE_LOOP('',(#19786,#19787,#19788,#19789,#19790,#19791));
#3747=EDGE_LOOP('',(#19792,#19793,#19794,#19795,#19796,#19797));
#3748=EDGE_LOOP('',(#19798,#19799,#19800,#19801));
#3749=EDGE_LOOP('',(#19802,#19803,#19804,#19805));
#3750=EDGE_LOOP('',(#19806,#19807,#19808,#19809));
#3751=EDGE_LOOP('',(#19810,#19811,#19812,#19813));
#3752=EDGE_LOOP('',(#19814,#19815,#19816,#19817));
#3753=EDGE_LOOP('',(#19818,#19819,#19820,#19821));
#3754=EDGE_LOOP('',(#19822,#19823,#19824,#19825));
#3755=EDGE_LOOP('',(#19826,#19827,#19828,#19829));
#3756=EDGE_LOOP('',(#19830,#19831,#19832,#19833));
#3757=EDGE_LOOP('',(#19834,#19835,#19836,#19837));
#3758=EDGE_LOOP('',(#19838,#19839,#19840,#19841));
#3759=EDGE_LOOP('',(#19842,#19843,#19844,#19845));
#3760=EDGE_LOOP('',(#19846,#19847,#19848,#19849));
#3761=EDGE_LOOP('',(#19850,#19851,#19852,#19853));
#3762=EDGE_LOOP('',(#19854,#19855,#19856,#19857));
#3763=EDGE_LOOP('',(#19858,#19859,#19860,#19861));
#3764=EDGE_LOOP('',(#19862,#19863,#19864,#19865,#19866,#19867));
#3765=EDGE_LOOP('',(#19868,#19869,#19870,#19871));
#3766=EDGE_LOOP('',(#19872,#19873,#19874,#19875,#19876,#19877));
#3767=EDGE_LOOP('',(#19878,#19879,#19880,#19881,#19882,#19883));
#3768=EDGE_LOOP('',(#19884,#19885,#19886,#19887));
#3769=EDGE_LOOP('',(#19888,#19889,#19890,#19891));
#3770=EDGE_LOOP('',(#19892,#19893,#19894,#19895));
#3771=EDGE_LOOP('',(#19896,#19897,#19898,#19899));
#3772=EDGE_LOOP('',(#19900,#19901,#19902,#19903));
#3773=EDGE_LOOP('',(#19904,#19905,#19906,#19907));
#3774=EDGE_LOOP('',(#19908,#19909,#19910,#19911));
#3775=EDGE_LOOP('',(#19912,#19913,#19914,#19915));
#3776=EDGE_LOOP('',(#19916,#19917,#19918,#19919));
#3777=EDGE_LOOP('',(#19920,#19921,#19922,#19923));
#3778=EDGE_LOOP('',(#19924,#19925,#19926,#19927));
#3779=EDGE_LOOP('',(#19928,#19929,#19930,#19931));
#3780=EDGE_LOOP('',(#19932,#19933,#19934,#19935));
#3781=EDGE_LOOP('',(#19936,#19937,#19938,#19939));
#3782=EDGE_LOOP('',(#19940,#19941,#19942,#19943));
#3783=EDGE_LOOP('',(#19944,#19945,#19946,#19947));
#3784=EDGE_LOOP('',(#19948,#19949,#19950,#19951,#19952,#19953));
#3785=EDGE_LOOP('',(#19954,#19955,#19956,#19957));
#3786=EDGE_LOOP('',(#19958,#19959,#19960,#19961,#19962,#19963));
#3787=EDGE_LOOP('',(#19964,#19965,#19966,#19967));
#3788=EDGE_LOOP('',(#19968));
#3789=EDGE_LOOP('',(#19969,#19970,#19971,#19972));
#3790=EDGE_LOOP('',(#19973,#19974,#19975,#19976));
#3791=EDGE_LOOP('',(#19977,#19978,#19979,#19980));
#3792=EDGE_LOOP('',(#19981));
#3793=EDGE_LOOP('',(#19982));
#3794=EDGE_LOOP('',(#19983,#19984,#19985,#19986));
#3795=EDGE_LOOP('',(#19987));
#3796=EDGE_LOOP('',(#19988,#19989,#19990,#19991,#19992,#19993));
#3797=EDGE_LOOP('',(#19994,#19995,#19996,#19997,#19998,#19999,#20000,#20001,
#20002,#20003,#20004,#20005,#20006,#20007,#20008,#20009,#20010,#20011,#20012,
#20013,#20014,#20015,#20016,#20017,#20018,#20019,#20020,#20021,#20022,#20023,
#20024,#20025,#20026,#20027,#20028,#20029,#20030,#20031,#20032,#20033,#20034,
#20035,#20036,#20037,#20038,#20039,#20040,#20041,#20042,#20043,#20044,#20045,
#20046,#20047,#20048,#20049,#20050,#20051,#20052,#20053,#20054,#20055,#20056,
#20057,#20058,#20059,#20060,#20061,#20062,#20063,#20064,#20065,#20066,#20067,
#20068,#20069,#20070,#20071,#20072,#20073,#20074,#20075,#20076,#20077,#20078,
#20079,#20080,#20081,#20082,#20083,#20084,#20085,#20086,#20087,#20088,#20089,
#20090,#20091,#20092,#20093,#20094,#20095,#20096,#20097,#20098,#20099,#20100,
#20101,#20102,#20103,#20104,#20105,#20106,#20107,#20108,#20109,#20110,#20111,
#20112,#20113,#20114,#20115,#20116,#20117,#20118,#20119,#20120,#20121,#20122,
#20123,#20124,#20125,#20126,#20127,#20128,#20129,#20130,#20131,#20132,#20133,
#20134,#20135,#20136,#20137,#20138,#20139,#20140,#20141,#20142,#20143,#20144,
#20145,#20146,#20147,#20148,#20149,#20150,#20151,#20152,#20153,#20154,#20155,
#20156,#20157,#20158,#20159,#20160,#20161,#20162,#20163,#20164,#20165,#20166,
#20167,#20168,#20169,#20170,#20171,#20172,#20173,#20174,#20175,#20176,#20177,
#20178,#20179,#20180,#20181,#20182,#20183,#20184,#20185,#20186,#20187,#20188,
#20189,#20190,#20191,#20192,#20193,#20194,#20195,#20196,#20197,#20198,#20199,
#20200,#20201,#20202,#20203,#20204,#20205,#20206,#20207,#20208,#20209,#20210,
#20211,#20212,#20213,#20214,#20215,#20216,#20217,#20218,#20219,#20220,#20221,
#20222,#20223,#20224,#20225,#20226,#20227,#20228,#20229,#20230,#20231,#20232,
#20233));
#3798=EDGE_LOOP('',(#20234));
#3799=EDGE_LOOP('',(#20235,#20236,#20237,#20238,#20239,#20240));
#3800=EDGE_LOOP('',(#20241,#20242,#20243,#20244));
#3801=EDGE_LOOP('',(#20245,#20246,#20247,#20248,#20249,#20250));
#3802=EDGE_LOOP('',(#20251,#20252,#20253,#20254,#20255,#20256));
#3803=EDGE_LOOP('',(#20257,#20258,#20259,#20260));
#3804=EDGE_LOOP('',(#20261,#20262,#20263,#20264,#20265,#20266));
#3805=EDGE_LOOP('',(#20267,#20268,#20269,#20270,#20271,#20272));
#3806=EDGE_LOOP('',(#20273,#20274,#20275,#20276));
#3807=EDGE_LOOP('',(#20277,#20278,#20279,#20280,#20281,#20282));
#3808=EDGE_LOOP('',(#20283,#20284,#20285,#20286,#20287,#20288));
#3809=EDGE_LOOP('',(#20289,#20290,#20291,#20292));
#3810=EDGE_LOOP('',(#20293,#20294,#20295,#20296,#20297,#20298));
#3811=EDGE_LOOP('',(#20299,#20300,#20301,#20302,#20303,#20304));
#3812=EDGE_LOOP('',(#20305,#20306,#20307,#20308));
#3813=EDGE_LOOP('',(#20309,#20310,#20311,#20312,#20313,#20314));
#3814=EDGE_LOOP('',(#20315,#20316,#20317,#20318,#20319,#20320));
#3815=EDGE_LOOP('',(#20321,#20322,#20323,#20324));
#3816=EDGE_LOOP('',(#20325,#20326,#20327,#20328,#20329,#20330));
#3817=EDGE_LOOP('',(#20331,#20332,#20333,#20334,#20335,#20336));
#3818=EDGE_LOOP('',(#20337,#20338,#20339,#20340));
#3819=EDGE_LOOP('',(#20341,#20342,#20343,#20344,#20345,#20346));
#3820=EDGE_LOOP('',(#20347,#20348,#20349,#20350,#20351,#20352));
#3821=EDGE_LOOP('',(#20353,#20354,#20355,#20356));
#3822=EDGE_LOOP('',(#20357,#20358,#20359,#20360,#20361,#20362));
#3823=EDGE_LOOP('',(#20363,#20364,#20365,#20366,#20367,#20368));
#3824=EDGE_LOOP('',(#20369,#20370,#20371,#20372));
#3825=EDGE_LOOP('',(#20373,#20374,#20375,#20376,#20377,#20378));
#3826=EDGE_LOOP('',(#20379,#20380,#20381,#20382,#20383,#20384));
#3827=EDGE_LOOP('',(#20385,#20386,#20387,#20388));
#3828=EDGE_LOOP('',(#20389,#20390,#20391,#20392,#20393,#20394));
#3829=EDGE_LOOP('',(#20395,#20396,#20397,#20398,#20399,#20400));
#3830=EDGE_LOOP('',(#20401,#20402,#20403,#20404));
#3831=EDGE_LOOP('',(#20405,#20406,#20407,#20408,#20409,#20410));
#3832=EDGE_LOOP('',(#20411,#20412,#20413,#20414,#20415,#20416));
#3833=EDGE_LOOP('',(#20417,#20418,#20419,#20420));
#3834=EDGE_LOOP('',(#20421,#20422,#20423,#20424,#20425,#20426));
#3835=EDGE_LOOP('',(#20427,#20428,#20429,#20430));
#3836=EDGE_LOOP('',(#20431,#20432,#20433,#20434));
#3837=EDGE_LOOP('',(#20435,#20436,#20437,#20438,#20439,#20440));
#3838=EDGE_LOOP('',(#20441,#20442,#20443,#20444));
#3839=EDGE_LOOP('',(#20445,#20446,#20447,#20448));
#3840=EDGE_LOOP('',(#20449,#20450,#20451,#20452,#20453,#20454));
#3841=EDGE_LOOP('',(#20455,#20456,#20457,#20458));
#3842=EDGE_LOOP('',(#20459,#20460,#20461,#20462));
#3843=EDGE_LOOP('',(#20463,#20464,#20465,#20466,#20467,#20468));
#3844=EDGE_LOOP('',(#20469,#20470,#20471,#20472));
#3845=EDGE_LOOP('',(#20473,#20474,#20475,#20476));
#3846=EDGE_LOOP('',(#20477,#20478,#20479,#20480,#20481,#20482));
#3847=EDGE_LOOP('',(#20483,#20484,#20485,#20486));
#3848=EDGE_LOOP('',(#20487,#20488,#20489,#20490));
#3849=EDGE_LOOP('',(#20491,#20492,#20493,#20494,#20495,#20496));
#3850=EDGE_LOOP('',(#20497,#20498,#20499,#20500));
#3851=EDGE_LOOP('',(#20501,#20502,#20503,#20504));
#3852=EDGE_LOOP('',(#20505,#20506,#20507,#20508,#20509,#20510));
#3853=EDGE_LOOP('',(#20511,#20512,#20513,#20514));
#3854=EDGE_LOOP('',(#20515,#20516,#20517,#20518));
#3855=EDGE_LOOP('',(#20519,#20520,#20521,#20522,#20523,#20524));
#3856=EDGE_LOOP('',(#20525,#20526,#20527,#20528));
#3857=EDGE_LOOP('',(#20529,#20530,#20531,#20532));
#3858=EDGE_LOOP('',(#20533,#20534,#20535,#20536,#20537,#20538));
#3859=EDGE_LOOP('',(#20539,#20540,#20541,#20542));
#3860=EDGE_LOOP('',(#20543,#20544,#20545,#20546));
#3861=EDGE_LOOP('',(#20547,#20548,#20549,#20550,#20551,#20552));
#3862=EDGE_LOOP('',(#20553,#20554,#20555,#20556));
#3863=EDGE_LOOP('',(#20557,#20558,#20559,#20560));
#3864=EDGE_LOOP('',(#20561,#20562,#20563,#20564,#20565,#20566));
#3865=EDGE_LOOP('',(#20567,#20568,#20569,#20570));
#3866=EDGE_LOOP('',(#20571,#20572,#20573,#20574));
#3867=EDGE_LOOP('',(#20575,#20576,#20577,#20578,#20579,#20580));
#3868=EDGE_LOOP('',(#20581,#20582,#20583,#20584));
#3869=EDGE_LOOP('',(#20585,#20586,#20587,#20588));
#3870=EDGE_LOOP('',(#20589,#20590,#20591,#20592,#20593,#20594));
#3871=EDGE_LOOP('',(#20595,#20596,#20597,#20598,#20599,#20600,#20601,#20602,
#20603,#20604,#20605,#20606,#20607,#20608,#20609,#20610,#20611,#20612,#20613,
#20614,#20615,#20616,#20617,#20618,#20619,#20620,#20621,#20622,#20623,#20624,
#20625,#20626,#20627,#20628,#20629,#20630,#20631,#20632,#20633,#20634,#20635,
#20636,#20637,#20638,#20639,#20640,#20641,#20642,#20643,#20644,#20645,#20646,
#20647,#20648,#20649,#20650,#20651,#20652,#20653,#20654,#20655,#20656,#20657,
#20658,#20659,#20660,#20661,#20662,#20663,#20664,#20665,#20666,#20667,#20668,
#20669,#20670,#20671,#20672,#20673,#20674,#20675,#20676,#20677,#20678,#20679,
#20680,#20681,#20682,#20683,#20684,#20685,#20686,#20687,#20688,#20689,#20690,
#20691,#20692,#20693,#20694,#20695,#20696,#20697,#20698,#20699,#20700,#20701,
#20702,#20703,#20704,#20705,#20706,#20707,#20708,#20709,#20710,#20711,#20712,
#20713,#20714,#20715,#20716,#20717,#20718,#20719,#20720,#20721,#20722,#20723,
#20724,#20725,#20726,#20727,#20728,#20729,#20730,#20731,#20732,#20733,#20734,
#20735,#20736,#20737,#20738,#20739,#20740,#20741,#20742,#20743,#20744,#20745,
#20746,#20747,#20748,#20749,#20750,#20751,#20752,#20753,#20754,#20755,#20756,
#20757,#20758,#20759,#20760,#20761,#20762,#20763,#20764,#20765,#20766,#20767,
#20768,#20769,#20770,#20771,#20772,#20773,#20774,#20775,#20776,#20777,#20778,
#20779,#20780,#20781,#20782,#20783,#20784,#20785,#20786,#20787,#20788,#20789,
#20790,#20791,#20792,#20793,#20794,#20795,#20796,#20797,#20798,#20799,#20800,
#20801,#20802,#20803,#20804,#20805,#20806,#20807,#20808,#20809,#20810,#20811,
#20812,#20813,#20814,#20815,#20816,#20817,#20818,#20819,#20820,#20821,#20822,
#20823,#20824,#20825,#20826,#20827,#20828,#20829,#20830,#20831,#20832,#20833,
#20834));
#3872=EDGE_LOOP('',(#20835));
#3873=EDGE_LOOP('',(#20836,#20837,#20838,#20839,#20840,#20841));
#3874=EDGE_LOOP('',(#20842,#20843,#20844,#20845,#20846,#20847));
#3875=EDGE_LOOP('',(#20848,#20849,#20850,#20851,#20852,#20853));
#3876=EDGE_LOOP('',(#20854,#20855,#20856,#20857,#20858,#20859));
#3877=EDGE_LOOP('',(#20860,#20861,#20862,#20863,#20864,#20865));
#3878=EDGE_LOOP('',(#20866,#20867,#20868,#20869,#20870,#20871));
#3879=EDGE_LOOP('',(#20872,#20873,#20874,#20875,#20876,#20877));
#3880=EDGE_LOOP('',(#20878,#20879,#20880,#20881,#20882,#20883));
#3881=EDGE_LOOP('',(#20884,#20885,#20886,#20887,#20888,#20889));
#3882=EDGE_LOOP('',(#20890,#20891,#20892,#20893,#20894,#20895));
#3883=EDGE_LOOP('',(#20896,#20897,#20898,#20899,#20900,#20901));
#3884=EDGE_LOOP('',(#20902,#20903,#20904,#20905,#20906,#20907));
#3885=EDGE_LOOP('',(#20908,#20909,#20910,#20911,#20912,#20913));
#3886=EDGE_LOOP('',(#20914,#20915,#20916,#20917,#20918,#20919));
#3887=EDGE_LOOP('',(#20920,#20921,#20922,#20923,#20924,#20925));
#3888=EDGE_LOOP('',(#20926,#20927,#20928,#20929,#20930,#20931));
#3889=EDGE_LOOP('',(#20932,#20933,#20934,#20935,#20936,#20937));
#3890=EDGE_LOOP('',(#20938,#20939,#20940,#20941,#20942,#20943));
#3891=EDGE_LOOP('',(#20944,#20945,#20946,#20947,#20948,#20949));
#3892=EDGE_LOOP('',(#20950,#20951,#20952,#20953,#20954,#20955));
#3893=EDGE_LOOP('',(#20956,#20957,#20958,#20959,#20960,#20961));
#3894=EDGE_LOOP('',(#20962,#20963,#20964,#20965,#20966,#20967));
#3895=EDGE_LOOP('',(#20968,#20969,#20970,#20971,#20972,#20973));
#3896=EDGE_LOOP('',(#20974,#20975,#20976,#20977,#20978,#20979));
#3897=EDGE_LOOP('',(#20980,#20981,#20982,#20983));
#3898=EDGE_LOOP('',(#20984,#20985,#20986,#20987));
#3899=EDGE_LOOP('',(#20988,#20989,#20990,#20991));
#3900=EDGE_LOOP('',(#20992,#20993,#20994,#20995));
#3901=EDGE_LOOP('',(#20996,#20997,#20998,#20999));
#3902=EDGE_LOOP('',(#21000,#21001,#21002,#21003));
#3903=EDGE_LOOP('',(#21004,#21005,#21006,#21007));
#3904=EDGE_LOOP('',(#21008,#21009,#21010,#21011));
#3905=EDGE_LOOP('',(#21012,#21013,#21014,#21015));
#3906=EDGE_LOOP('',(#21016,#21017,#21018,#21019));
#3907=EDGE_LOOP('',(#21020,#21021,#21022,#21023));
#3908=EDGE_LOOP('',(#21024,#21025,#21026,#21027));
#3909=EDGE_LOOP('',(#21028,#21029,#21030,#21031));
#3910=EDGE_LOOP('',(#21032,#21033,#21034,#21035));
#3911=EDGE_LOOP('',(#21036,#21037,#21038,#21039));
#3912=EDGE_LOOP('',(#21040,#21041,#21042,#21043));
#3913=EDGE_LOOP('',(#21044,#21045,#21046,#21047,#21048,#21049));
#3914=EDGE_LOOP('',(#21050,#21051,#21052,#21053));
#3915=EDGE_LOOP('',(#21054,#21055,#21056,#21057,#21058,#21059));
#3916=EDGE_LOOP('',(#21060,#21061,#21062,#21063,#21064,#21065));
#3917=EDGE_LOOP('',(#21066,#21067,#21068,#21069));
#3918=EDGE_LOOP('',(#21070,#21071,#21072,#21073));
#3919=EDGE_LOOP('',(#21074,#21075,#21076,#21077));
#3920=EDGE_LOOP('',(#21078,#21079,#21080,#21081));
#3921=EDGE_LOOP('',(#21082,#21083,#21084,#21085));
#3922=EDGE_LOOP('',(#21086,#21087,#21088,#21089));
#3923=EDGE_LOOP('',(#21090,#21091,#21092,#21093));
#3924=EDGE_LOOP('',(#21094,#21095,#21096,#21097));
#3925=EDGE_LOOP('',(#21098,#21099,#21100,#21101));
#3926=EDGE_LOOP('',(#21102,#21103,#21104,#21105));
#3927=EDGE_LOOP('',(#21106,#21107,#21108,#21109));
#3928=EDGE_LOOP('',(#21110,#21111,#21112,#21113));
#3929=EDGE_LOOP('',(#21114,#21115,#21116,#21117));
#3930=EDGE_LOOP('',(#21118,#21119,#21120,#21121));
#3931=EDGE_LOOP('',(#21122,#21123,#21124,#21125));
#3932=EDGE_LOOP('',(#21126,#21127,#21128,#21129));
#3933=EDGE_LOOP('',(#21130,#21131,#21132,#21133,#21134,#21135));
#3934=EDGE_LOOP('',(#21136,#21137,#21138,#21139));
#3935=EDGE_LOOP('',(#21140,#21141,#21142,#21143,#21144,#21145));
#3936=EDGE_LOOP('',(#21146,#21147,#21148,#21149,#21150,#21151));
#3937=EDGE_LOOP('',(#21152,#21153,#21154,#21155));
#3938=EDGE_LOOP('',(#21156,#21157,#21158,#21159));
#3939=EDGE_LOOP('',(#21160,#21161,#21162,#21163));
#3940=EDGE_LOOP('',(#21164,#21165,#21166,#21167));
#3941=EDGE_LOOP('',(#21168,#21169,#21170,#21171));
#3942=EDGE_LOOP('',(#21172,#21173,#21174,#21175));
#3943=EDGE_LOOP('',(#21176,#21177,#21178,#21179));
#3944=EDGE_LOOP('',(#21180,#21181,#21182,#21183));
#3945=EDGE_LOOP('',(#21184,#21185,#21186,#21187));
#3946=EDGE_LOOP('',(#21188,#21189,#21190,#21191));
#3947=EDGE_LOOP('',(#21192,#21193,#21194,#21195));
#3948=EDGE_LOOP('',(#21196,#21197,#21198,#21199));
#3949=EDGE_LOOP('',(#21200,#21201,#21202,#21203));
#3950=EDGE_LOOP('',(#21204,#21205,#21206,#21207));
#3951=EDGE_LOOP('',(#21208,#21209,#21210,#21211));
#3952=EDGE_LOOP('',(#21212,#21213,#21214,#21215));
#3953=EDGE_LOOP('',(#21216,#21217,#21218,#21219,#21220,#21221));
#3954=EDGE_LOOP('',(#21222,#21223,#21224,#21225));
#3955=EDGE_LOOP('',(#21226,#21227,#21228,#21229,#21230,#21231));
#3956=EDGE_LOOP('',(#21232,#21233,#21234,#21235,#21236,#21237));
#3957=EDGE_LOOP('',(#21238,#21239,#21240,#21241));
#3958=EDGE_LOOP('',(#21242,#21243,#21244,#21245));
#3959=EDGE_LOOP('',(#21246,#21247,#21248,#21249));
#3960=EDGE_LOOP('',(#21250,#21251,#21252,#21253));
#3961=EDGE_LOOP('',(#21254,#21255,#21256,#21257));
#3962=EDGE_LOOP('',(#21258,#21259,#21260,#21261));
#3963=EDGE_LOOP('',(#21262,#21263,#21264,#21265));
#3964=EDGE_LOOP('',(#21266,#21267,#21268,#21269));
#3965=EDGE_LOOP('',(#21270,#21271,#21272,#21273));
#3966=EDGE_LOOP('',(#21274,#21275,#21276,#21277));
#3967=EDGE_LOOP('',(#21278,#21279,#21280,#21281));
#3968=EDGE_LOOP('',(#21282,#21283,#21284,#21285));
#3969=EDGE_LOOP('',(#21286,#21287,#21288,#21289));
#3970=EDGE_LOOP('',(#21290,#21291,#21292,#21293));
#3971=EDGE_LOOP('',(#21294,#21295,#21296,#21297));
#3972=EDGE_LOOP('',(#21298,#21299,#21300,#21301));
#3973=EDGE_LOOP('',(#21302,#21303,#21304,#21305,#21306,#21307));
#3974=EDGE_LOOP('',(#21308,#21309,#21310,#21311));
#3975=EDGE_LOOP('',(#21312,#21313,#21314,#21315,#21316,#21317));
#3976=EDGE_LOOP('',(#21318,#21319,#21320,#21321,#21322,#21323));
#3977=EDGE_LOOP('',(#21324,#21325,#21326,#21327));
#3978=EDGE_LOOP('',(#21328,#21329,#21330,#21331));
#3979=EDGE_LOOP('',(#21332,#21333,#21334,#21335));
#3980=EDGE_LOOP('',(#21336,#21337,#21338,#21339));
#3981=EDGE_LOOP('',(#21340,#21341,#21342,#21343));
#3982=EDGE_LOOP('',(#21344,#21345,#21346,#21347));
#3983=EDGE_LOOP('',(#21348,#21349,#21350,#21351));
#3984=EDGE_LOOP('',(#21352,#21353,#21354,#21355));
#3985=EDGE_LOOP('',(#21356,#21357,#21358,#21359));
#3986=EDGE_LOOP('',(#21360,#21361,#21362,#21363));
#3987=EDGE_LOOP('',(#21364,#21365,#21366,#21367));
#3988=EDGE_LOOP('',(#21368,#21369,#21370,#21371));
#3989=EDGE_LOOP('',(#21372,#21373,#21374,#21375));
#3990=EDGE_LOOP('',(#21376,#21377,#21378,#21379));
#3991=EDGE_LOOP('',(#21380,#21381,#21382,#21383));
#3992=EDGE_LOOP('',(#21384,#21385,#21386,#21387));
#3993=EDGE_LOOP('',(#21388,#21389,#21390,#21391,#21392,#21393));
#3994=EDGE_LOOP('',(#21394,#21395,#21396,#21397));
#3995=EDGE_LOOP('',(#21398,#21399,#21400,#21401,#21402,#21403));
#3996=EDGE_LOOP('',(#21404,#21405,#21406,#21407,#21408,#21409));
#3997=EDGE_LOOP('',(#21410,#21411,#21412,#21413));
#3998=EDGE_LOOP('',(#21414,#21415,#21416,#21417));
#3999=EDGE_LOOP('',(#21418,#21419,#21420,#21421));
#4000=EDGE_LOOP('',(#21422,#21423,#21424,#21425));
#4001=EDGE_LOOP('',(#21426,#21427,#21428,#21429));
#4002=EDGE_LOOP('',(#21430,#21431,#21432,#21433));
#4003=EDGE_LOOP('',(#21434,#21435,#21436,#21437));
#4004=EDGE_LOOP('',(#21438,#21439,#21440,#21441));
#4005=EDGE_LOOP('',(#21442,#21443,#21444,#21445));
#4006=EDGE_LOOP('',(#21446,#21447,#21448,#21449));
#4007=EDGE_LOOP('',(#21450,#21451,#21452,#21453));
#4008=EDGE_LOOP('',(#21454,#21455,#21456,#21457));
#4009=EDGE_LOOP('',(#21458,#21459,#21460,#21461));
#4010=EDGE_LOOP('',(#21462,#21463,#21464,#21465));
#4011=EDGE_LOOP('',(#21466,#21467,#21468,#21469));
#4012=EDGE_LOOP('',(#21470,#21471,#21472,#21473));
#4013=EDGE_LOOP('',(#21474,#21475,#21476,#21477,#21478,#21479));
#4014=EDGE_LOOP('',(#21480,#21481,#21482,#21483));
#4015=EDGE_LOOP('',(#21484,#21485,#21486,#21487,#21488,#21489));
#4016=EDGE_LOOP('',(#21490,#21491,#21492,#21493,#21494,#21495));
#4017=EDGE_LOOP('',(#21496,#21497,#21498,#21499));
#4018=EDGE_LOOP('',(#21500,#21501,#21502,#21503));
#4019=EDGE_LOOP('',(#21504,#21505,#21506,#21507));
#4020=EDGE_LOOP('',(#21508,#21509,#21510,#21511));
#4021=EDGE_LOOP('',(#21512,#21513,#21514,#21515));
#4022=EDGE_LOOP('',(#21516,#21517,#21518,#21519));
#4023=EDGE_LOOP('',(#21520,#21521,#21522,#21523));
#4024=EDGE_LOOP('',(#21524,#21525,#21526,#21527));
#4025=EDGE_LOOP('',(#21528,#21529,#21530,#21531));
#4026=EDGE_LOOP('',(#21532,#21533,#21534,#21535));
#4027=EDGE_LOOP('',(#21536,#21537,#21538,#21539));
#4028=EDGE_LOOP('',(#21540,#21541,#21542,#21543));
#4029=EDGE_LOOP('',(#21544,#21545,#21546,#21547));
#4030=EDGE_LOOP('',(#21548,#21549,#21550,#21551));
#4031=EDGE_LOOP('',(#21552,#21553,#21554,#21555));
#4032=EDGE_LOOP('',(#21556,#21557,#21558,#21559));
#4033=EDGE_LOOP('',(#21560,#21561,#21562,#21563,#21564,#21565));
#4034=EDGE_LOOP('',(#21566,#21567,#21568,#21569));
#4035=EDGE_LOOP('',(#21570,#21571,#21572,#21573,#21574,#21575));
#4036=EDGE_LOOP('',(#21576,#21577,#21578,#21579,#21580,#21581));
#4037=EDGE_LOOP('',(#21582,#21583,#21584,#21585));
#4038=EDGE_LOOP('',(#21586,#21587,#21588,#21589));
#4039=EDGE_LOOP('',(#21590,#21591,#21592,#21593));
#4040=EDGE_LOOP('',(#21594,#21595,#21596,#21597));
#4041=EDGE_LOOP('',(#21598,#21599,#21600,#21601));
#4042=EDGE_LOOP('',(#21602,#21603,#21604,#21605));
#4043=EDGE_LOOP('',(#21606,#21607,#21608,#21609));
#4044=EDGE_LOOP('',(#21610,#21611,#21612,#21613));
#4045=EDGE_LOOP('',(#21614,#21615,#21616,#21617));
#4046=EDGE_LOOP('',(#21618,#21619,#21620,#21621));
#4047=EDGE_LOOP('',(#21622,#21623,#21624,#21625));
#4048=EDGE_LOOP('',(#21626,#21627,#21628,#21629));
#4049=EDGE_LOOP('',(#21630,#21631,#21632,#21633));
#4050=EDGE_LOOP('',(#21634,#21635,#21636,#21637));
#4051=EDGE_LOOP('',(#21638,#21639,#21640,#21641));
#4052=EDGE_LOOP('',(#21642,#21643,#21644,#21645));
#4053=EDGE_LOOP('',(#21646,#21647,#21648,#21649,#21650,#21651));
#4054=EDGE_LOOP('',(#21652,#21653,#21654,#21655));
#4055=EDGE_LOOP('',(#21656,#21657,#21658,#21659,#21660,#21661));
#4056=EDGE_LOOP('',(#21662,#21663,#21664,#21665,#21666,#21667));
#4057=EDGE_LOOP('',(#21668,#21669,#21670,#21671));
#4058=EDGE_LOOP('',(#21672,#21673,#21674,#21675));
#4059=EDGE_LOOP('',(#21676,#21677,#21678,#21679));
#4060=EDGE_LOOP('',(#21680,#21681,#21682,#21683));
#4061=EDGE_LOOP('',(#21684,#21685,#21686,#21687));
#4062=EDGE_LOOP('',(#21688,#21689,#21690,#21691));
#4063=EDGE_LOOP('',(#21692,#21693,#21694,#21695));
#4064=EDGE_LOOP('',(#21696,#21697,#21698,#21699));
#4065=EDGE_LOOP('',(#21700,#21701,#21702,#21703));
#4066=EDGE_LOOP('',(#21704,#21705,#21706,#21707));
#4067=EDGE_LOOP('',(#21708,#21709,#21710,#21711));
#4068=EDGE_LOOP('',(#21712,#21713,#21714,#21715));
#4069=EDGE_LOOP('',(#21716,#21717,#21718,#21719));
#4070=EDGE_LOOP('',(#21720,#21721,#21722,#21723));
#4071=EDGE_LOOP('',(#21724,#21725,#21726,#21727));
#4072=EDGE_LOOP('',(#21728,#21729,#21730,#21731));
#4073=EDGE_LOOP('',(#21732,#21733,#21734,#21735,#21736,#21737));
#4074=EDGE_LOOP('',(#21738,#21739,#21740,#21741));
#4075=EDGE_LOOP('',(#21742,#21743,#21744,#21745,#21746,#21747));
#4076=EDGE_LOOP('',(#21748,#21749,#21750,#21751,#21752,#21753));
#4077=EDGE_LOOP('',(#21754,#21755,#21756,#21757));
#4078=EDGE_LOOP('',(#21758,#21759,#21760,#21761));
#4079=EDGE_LOOP('',(#21762,#21763,#21764,#21765));
#4080=EDGE_LOOP('',(#21766,#21767,#21768,#21769));
#4081=EDGE_LOOP('',(#21770,#21771,#21772,#21773));
#4082=EDGE_LOOP('',(#21774,#21775,#21776,#21777));
#4083=EDGE_LOOP('',(#21778,#21779,#21780,#21781));
#4084=EDGE_LOOP('',(#21782,#21783,#21784,#21785));
#4085=EDGE_LOOP('',(#21786,#21787,#21788,#21789));
#4086=EDGE_LOOP('',(#21790,#21791,#21792,#21793));
#4087=EDGE_LOOP('',(#21794,#21795,#21796,#21797));
#4088=EDGE_LOOP('',(#21798,#21799,#21800,#21801));
#4089=EDGE_LOOP('',(#21802,#21803,#21804,#21805));
#4090=EDGE_LOOP('',(#21806,#21807,#21808,#21809));
#4091=EDGE_LOOP('',(#21810,#21811,#21812,#21813));
#4092=EDGE_LOOP('',(#21814,#21815,#21816,#21817));
#4093=EDGE_LOOP('',(#21818,#21819,#21820,#21821,#21822,#21823));
#4094=EDGE_LOOP('',(#21824,#21825,#21826,#21827));
#4095=EDGE_LOOP('',(#21828,#21829,#21830,#21831,#21832,#21833));
#4096=EDGE_LOOP('',(#21834,#21835,#21836,#21837,#21838,#21839));
#4097=EDGE_LOOP('',(#21840,#21841,#21842,#21843));
#4098=EDGE_LOOP('',(#21844,#21845,#21846,#21847));
#4099=EDGE_LOOP('',(#21848,#21849,#21850,#21851));
#4100=EDGE_LOOP('',(#21852,#21853,#21854,#21855));
#4101=EDGE_LOOP('',(#21856,#21857,#21858,#21859));
#4102=EDGE_LOOP('',(#21860,#21861,#21862,#21863));
#4103=EDGE_LOOP('',(#21864,#21865,#21866,#21867));
#4104=EDGE_LOOP('',(#21868,#21869,#21870,#21871));
#4105=EDGE_LOOP('',(#21872,#21873,#21874,#21875));
#4106=EDGE_LOOP('',(#21876,#21877,#21878,#21879));
#4107=EDGE_LOOP('',(#21880,#21881,#21882,#21883));
#4108=EDGE_LOOP('',(#21884,#21885,#21886,#21887));
#4109=EDGE_LOOP('',(#21888,#21889,#21890,#21891));
#4110=EDGE_LOOP('',(#21892,#21893,#21894,#21895));
#4111=EDGE_LOOP('',(#21896,#21897,#21898,#21899));
#4112=EDGE_LOOP('',(#21900,#21901,#21902,#21903));
#4113=EDGE_LOOP('',(#21904,#21905,#21906,#21907,#21908,#21909));
#4114=EDGE_LOOP('',(#21910,#21911,#21912,#21913));
#4115=EDGE_LOOP('',(#21914,#21915,#21916,#21917,#21918,#21919));
#4116=EDGE_LOOP('',(#21920,#21921,#21922,#21923,#21924,#21925));
#4117=EDGE_LOOP('',(#21926,#21927,#21928,#21929));
#4118=EDGE_LOOP('',(#21930,#21931,#21932,#21933));
#4119=EDGE_LOOP('',(#21934,#21935,#21936,#21937));
#4120=EDGE_LOOP('',(#21938,#21939,#21940,#21941));
#4121=EDGE_LOOP('',(#21942,#21943,#21944,#21945));
#4122=EDGE_LOOP('',(#21946,#21947,#21948,#21949));
#4123=EDGE_LOOP('',(#21950,#21951,#21952,#21953));
#4124=EDGE_LOOP('',(#21954,#21955,#21956,#21957));
#4125=EDGE_LOOP('',(#21958,#21959,#21960,#21961));
#4126=EDGE_LOOP('',(#21962,#21963,#21964,#21965));
#4127=EDGE_LOOP('',(#21966,#21967,#21968,#21969));
#4128=EDGE_LOOP('',(#21970,#21971,#21972,#21973));
#4129=EDGE_LOOP('',(#21974,#21975,#21976,#21977));
#4130=EDGE_LOOP('',(#21978,#21979,#21980,#21981));
#4131=EDGE_LOOP('',(#21982,#21983,#21984,#21985));
#4132=EDGE_LOOP('',(#21986,#21987,#21988,#21989));
#4133=EDGE_LOOP('',(#21990,#21991,#21992,#21993,#21994,#21995));
#4134=EDGE_LOOP('',(#21996,#21997,#21998,#21999));
#4135=EDGE_LOOP('',(#22000,#22001,#22002,#22003,#22004,#22005));
#4136=EDGE_LOOP('',(#22006,#22007,#22008,#22009));
#4137=EDGE_LOOP('',(#22010));
#4138=EDGE_LOOP('',(#22011,#22012,#22013,#22014));
#4139=EDGE_LOOP('',(#22015));
#4140=EDGE_LOOP('',(#22016,#22017,#22018,#22019));
#4141=EDGE_LOOP('',(#22020,#22021,#22022,#22023));
#4142=EDGE_LOOP('',(#22024,#22025,#22026,#22027));
#4143=EDGE_LOOP('',(#22028,#22029,#22030,#22031));
#4144=EDGE_LOOP('',(#22032,#22033,#22034,#22035));
#4145=EDGE_LOOP('',(#22036,#22037,#22038,#22039));
#4146=EDGE_LOOP('',(#22040,#22041,#22042,#22043));
#4147=EDGE_LOOP('',(#22044,#22045,#22046,#22047));
#4148=EDGE_LOOP('',(#22048,#22049,#22050,#22051));
#4149=EDGE_LOOP('',(#22052,#22053,#22054,#22055));
#4150=EDGE_LOOP('',(#22056,#22057,#22058,#22059));
#4151=EDGE_LOOP('',(#22060,#22061,#22062,#22063));
#4152=EDGE_LOOP('',(#22064,#22065,#22066,#22067));
#4153=EDGE_LOOP('',(#22068,#22069,#22070,#22071));
#4154=EDGE_LOOP('',(#22072,#22073));
#4155=EDGE_LOOP('',(#22074,#22075,#22076,#22077));
#4156=EDGE_LOOP('',(#22078,#22079,#22080,#22081));
#4157=EDGE_LOOP('',(#22082));
#4158=EDGE_LOOP('',(#22083));
#4159=EDGE_LOOP('',(#22084,#22085));
#4160=EDGE_LOOP('',(#22086));
#4161=EDGE_LOOP('',(#22087));
#4162=EDGE_LOOP('',(#22088,#22089,#22090,#22091,#22092));
#4163=EDGE_LOOP('',(#22093));
#4164=EDGE_LOOP('',(#22094));
#4165=EDGE_LOOP('',(#22095,#22096,#22097,#22098,#22099));
#4166=EDGE_LOOP('',(#22100,#22101,#22102,#22103));
#4167=EDGE_LOOP('',(#22104));
#4168=EDGE_LOOP('',(#22105));
#4169=EDGE_LOOP('',(#22106,#22107,#22108,#22109));
#4170=EDGE_LOOP('',(#22110));
#4171=EDGE_LOOP('',(#22111));
#4172=EDGE_LOOP('',(#22112,#22113,#22114,#22115));
#4173=EDGE_LOOP('',(#22116));
#4174=EDGE_LOOP('',(#22117));
#4175=EDGE_LOOP('',(#22118,#22119,#22120,#22121));
#4176=EDGE_LOOP('',(#22122,#22123,#22124,#22125));
#4177=EDGE_LOOP('',(#22126,#22127,#22128,#22129));
#4178=EDGE_LOOP('',(#22130,#22131,#22132,#22133));
#4179=EDGE_LOOP('',(#22134,#22135,#22136,#22137));
#4180=EDGE_LOOP('',(#22138,#22139,#22140,#22141));
#4181=EDGE_LOOP('',(#22142,#22143,#22144,#22145));
#4182=EDGE_LOOP('',(#22146,#22147,#22148,#22149));
#4183=EDGE_LOOP('',(#22150,#22151,#22152,#22153));
#4184=EDGE_LOOP('',(#22154,#22155,#22156,#22157));
#4185=EDGE_LOOP('',(#22158,#22159,#22160,#22161));
#4186=EDGE_LOOP('',(#22162));
#4187=EDGE_LOOP('',(#22163));
#4188=EDGE_LOOP('',(#22164,#22165,#22166,#22167,#22168,#22169,#22170,#22171));
#4189=EDGE_LOOP('',(#22172,#22173,#22174,#22175));
#4190=EDGE_LOOP('',(#22176,#22177,#22178,#22179));
#4191=EDGE_LOOP('',(#22180,#22181,#22182,#22183));
#4192=EDGE_LOOP('',(#22184,#22185,#22186,#22187));
#4193=EDGE_LOOP('',(#22188));
#4194=EDGE_LOOP('',(#22189));
#4195=EDGE_LOOP('',(#22190,#22191,#22192,#22193));
#4196=EDGE_LOOP('',(#22194,#22195,#22196,#22197));
#4197=EDGE_LOOP('',(#22198,#22199,#22200,#22201));
#4198=EDGE_LOOP('',(#22202,#22203,#22204,#22205,#22206,#22207));
#4199=EDGE_LOOP('',(#22208,#22209,#22210,#22211));
#4200=EDGE_LOOP('',(#22212,#22213,#22214,#22215,#22216,#22217));
#4201=EDGE_LOOP('',(#22218,#22219,#22220,#22221,#22222,#22223));
#4202=EDGE_LOOP('',(#22224,#22225,#22226,#22227,#22228,#22229));
#4203=EDGE_LOOP('',(#22230,#22231,#22232,#22233));
#4204=EDGE_LOOP('',(#22234,#22235,#22236,#22237,#22238,#22239));
#4205=EDGE_LOOP('',(#22240,#22241,#22242,#22243,#22244,#22245));
#4206=EDGE_LOOP('',(#22246,#22247,#22248,#22249));
#4207=EDGE_LOOP('',(#22250,#22251,#22252,#22253,#22254,#22255));
#4208=EDGE_LOOP('',(#22256,#22257,#22258,#22259,#22260,#22261));
#4209=EDGE_LOOP('',(#22262,#22263,#22264,#22265));
#4210=EDGE_LOOP('',(#22266,#22267,#22268,#22269,#22270,#22271));
#4211=EDGE_LOOP('',(#22272,#22273,#22274,#22275,#22276,#22277));
#4212=EDGE_LOOP('',(#22278,#22279,#22280,#22281,#22282,#22283));
#4213=EDGE_LOOP('',(#22284,#22285,#22286,#22287));
#4214=EDGE_LOOP('',(#22288,#22289,#22290,#22291,#22292,#22293));
#4215=EDGE_LOOP('',(#22294,#22295,#22296,#22297));
#4216=EDGE_LOOP('',(#22298,#22299,#22300,#22301,#22302,#22303));
#4217=EDGE_LOOP('',(#22304,#22305,#22306,#22307,#22308,#22309));
#4218=EDGE_LOOP('',(#22310,#22311,#22312,#22313,#22314,#22315));
#4219=EDGE_LOOP('',(#22316,#22317,#22318,#22319,#22320,#22321));
#4220=EDGE_LOOP('',(#22322,#22323,#22324));
#4221=EDGE_LOOP('',(#22325,#22326,#22327));
#4222=EDGE_LOOP('',(#22328,#22329,#22330));
#4223=EDGE_LOOP('',(#22331,#22332,#22333));
#4224=EDGE_LOOP('',(#22334,#22335,#22336,#22337));
#4225=EDGE_LOOP('',(#22338,#22339,#22340));
#4226=EDGE_LOOP('',(#22341,#22342,#22343));
#4227=EDGE_LOOP('',(#22344,#22345,#22346,#22347));
#4228=EDGE_LOOP('',(#22348,#22349,#22350,#22351));
#4229=EDGE_LOOP('',(#22352,#22353,#22354,#22355));
#4230=EDGE_LOOP('',(#22356,#22357,#22358,#22359));
#4231=EDGE_LOOP('',(#22360,#22361,#22362,#22363));
#4232=EDGE_LOOP('',(#22364,#22365,#22366,#22367));
#4233=EDGE_LOOP('',(#22368,#22369,#22370,#22371));
#4234=EDGE_LOOP('',(#22372,#22373,#22374,#22375));
#4235=EDGE_LOOP('',(#22376,#22377,#22378,#22379));
#4236=EDGE_LOOP('',(#22380,#22381,#22382,#22383));
#4237=EDGE_LOOP('',(#22384,#22385,#22386,#22387));
#4238=EDGE_LOOP('',(#22388,#22389,#22390,#22391));
#4239=EDGE_LOOP('',(#22392,#22393,#22394,#22395,#22396));
#4240=EDGE_LOOP('',(#22397,#22398,#22399,#22400));
#4241=EDGE_LOOP('',(#22401,#22402,#22403,#22404,#22405,#22406));
#4242=EDGE_LOOP('',(#22407));
#4243=EDGE_LOOP('',(#22408,#22409,#22410,#22411));
#4244=EDGE_LOOP('',(#22412,#22413,#22414,#22415));
#4245=EDGE_LOOP('',(#22416,#22417,#22418,#22419));
#4246=EDGE_LOOP('',(#22420,#22421,#22422,#22423));
#4247=EDGE_LOOP('',(#22424,#22425,#22426,#22427));
#4248=EDGE_LOOP('',(#22428,#22429,#22430,#22431));
#4249=EDGE_LOOP('',(#22432,#22433,#22434,#22435));
#4250=EDGE_LOOP('',(#22436,#22437,#22438,#22439));
#4251=EDGE_LOOP('',(#22440,#22441,#22442,#22443));
#4252=EDGE_LOOP('',(#22444));
#4253=EDGE_LOOP('',(#22445,#22446,#22447,#22448,#22449,#22450));
#4254=EDGE_LOOP('',(#22451,#22452,#22453,#22454));
#4255=EDGE_LOOP('',(#22455,#22456,#22457,#22458));
#4256=EDGE_LOOP('',(#22459,#22460,#22461,#22462));
#4257=EDGE_LOOP('',(#22463,#22464,#22465,#22466,#22467,#22468));
#4258=EDGE_LOOP('',(#22469,#22470,#22471,#22472,#22473,#22474,#22475,#22476,
#22477,#22478,#22479,#22480,#22481,#22482,#22483,#22484));
#4259=EDGE_LOOP('',(#22485,#22486,#22487,#22488));
#4260=EDGE_LOOP('',(#22489,#22490,#22491,#22492));
#4261=EDGE_LOOP('',(#22493,#22494,#22495,#22496));
#4262=EDGE_LOOP('',(#22497));
#4263=EDGE_LOOP('',(#22498,#22499,#22500,#22501));
#4264=EDGE_LOOP('',(#22502,#22503,#22504,#22505));
#4265=EDGE_LOOP('',(#22506));
#4266=EDGE_LOOP('',(#22507));
#4267=EDGE_LOOP('',(#22508,#22509,#22510,#22511));
#4268=EDGE_LOOP('',(#22512,#22513,#22514,#22515));
#4269=EDGE_LOOP('',(#22516));
#4270=EDGE_LOOP('',(#22517));
#4271=EDGE_LOOP('',(#22518));
#4272=EDGE_LOOP('',(#22519));
#4273=EDGE_LOOP('',(#22520,#22521,#22522,#22523));
#4274=EDGE_LOOP('',(#22524,#22525,#22526,#22527));
#4275=EDGE_LOOP('',(#22528));
#4276=EDGE_LOOP('',(#22529));
#4277=EDGE_LOOP('',(#22530,#22531,#22532,#22533));
#4278=EDGE_LOOP('',(#22534));
#4279=EDGE_LOOP('',(#22535));
#4280=EDGE_LOOP('',(#22536,#22537,#22538,#22539));
#4281=EDGE_LOOP('',(#22540));
#4282=EDGE_LOOP('',(#22541));
#4283=EDGE_LOOP('',(#22542,#22543,#22544,#22545));
#4284=EDGE_LOOP('',(#22546));
#4285=EDGE_LOOP('',(#22547));
#4286=EDGE_LOOP('',(#22548,#22549,#22550,#22551));
#4287=EDGE_LOOP('',(#22552,#22553,#22554,#22555));
#4288=EDGE_LOOP('',(#22556,#22557,#22558,#22559));
#4289=EDGE_LOOP('',(#22560,#22561,#22562,#22563));
#4290=EDGE_LOOP('',(#22564,#22565,#22566,#22567));
#4291=EDGE_LOOP('',(#22568,#22569,#22570,#22571));
#4292=EDGE_LOOP('',(#22572,#22573,#22574,#22575));
#4293=EDGE_LOOP('',(#22576,#22577,#22578,#22579));
#4294=EDGE_LOOP('',(#22580,#22581,#22582,#22583));
#4295=EDGE_LOOP('',(#22584,#22585,#22586,#22587));
#4296=EDGE_LOOP('',(#22588,#22589,#22590,#22591));
#4297=EDGE_LOOP('',(#22592,#22593,#22594,#22595));
#4298=EDGE_LOOP('',(#22596,#22597,#22598,#22599));
#4299=EDGE_LOOP('',(#22600,#22601,#22602,#22603));
#4300=EDGE_LOOP('',(#22604,#22605,#22606,#22607));
#4301=EDGE_LOOP('',(#22608,#22609,#22610,#22611));
#4302=EDGE_LOOP('',(#22612,#22613,#22614,#22615));
#4303=EDGE_LOOP('',(#22616,#22617,#22618,#22619));
#4304=EDGE_LOOP('',(#22620,#22621,#22622,#22623));
#4305=EDGE_LOOP('',(#22624,#22625,#22626,#22627));
#4306=EDGE_LOOP('',(#22628,#22629,#22630,#22631,#22632));
#4307=EDGE_LOOP('',(#22633,#22634,#22635,#22636));
#4308=EDGE_LOOP('',(#22637,#22638,#22639,#22640));
#4309=EDGE_LOOP('',(#22641,#22642,#22643,#22644));
#4310=EDGE_LOOP('',(#22645,#22646,#22647,#22648));
#4311=EDGE_LOOP('',(#22649,#22650,#22651,#22652));
#4312=EDGE_LOOP('',(#22653,#22654,#22655,#22656));
#4313=EDGE_LOOP('',(#22657,#22658,#22659,#22660));
#4314=EDGE_LOOP('',(#22661,#22662,#22663,#22664));
#4315=EDGE_LOOP('',(#22665,#22666,#22667,#22668));
#4316=EDGE_LOOP('',(#22669,#22670,#22671,#22672));
#4317=EDGE_LOOP('',(#22673,#22674,#22675,#22676));
#4318=EDGE_LOOP('',(#22677,#22678,#22679,#22680));
#4319=EDGE_LOOP('',(#22681,#22682,#22683,#22684));
#4320=EDGE_LOOP('',(#22685,#22686,#22687,#22688));
#4321=EDGE_LOOP('',(#22689,#22690,#22691,#22692));
#4322=EDGE_LOOP('',(#22693,#22694,#22695,#22696));
#4323=EDGE_LOOP('',(#22697,#22698,#22699,#22700));
#4324=EDGE_LOOP('',(#22701,#22702,#22703,#22704));
#4325=EDGE_LOOP('',(#22705,#22706,#22707,#22708));
#4326=EDGE_LOOP('',(#22709,#22710,#22711,#22712));
#4327=EDGE_LOOP('',(#22713,#22714,#22715,#22716));
#4328=EDGE_LOOP('',(#22717,#22718,#22719,#22720,#22721,#22722,#22723,#22724,
#22725,#22726,#22727,#22728,#22729,#22730,#22731,#22732,#22733,#22734,#22735,
#22736,#22737,#22738,#22739,#22740,#22741,#22742,#22743,#22744,#22745,#22746,
#22747,#22748,#22749,#22750,#22751,#22752,#22753,#22754,#22755,#22756,#22757,
#22758,#22759,#22760,#22761));
#4329=EDGE_LOOP('',(#22762,#22763,#22764,#22765,#22766));
#4330=EDGE_LOOP('',(#22767,#22768,#22769,#22770));
#4331=EDGE_LOOP('',(#22771,#22772,#22773,#22774,#22775,#22776,#22777,#22778,
#22779,#22780,#22781,#22782,#22783,#22784,#22785,#22786,#22787,#22788,#22789,
#22790,#22791,#22792,#22793,#22794,#22795,#22796,#22797,#22798,#22799,#22800,
#22801,#22802,#22803,#22804,#22805,#22806,#22807,#22808,#22809,#22810,#22811,
#22812,#22813,#22814));
#4332=EDGE_LOOP('',(#22815,#22816,#22817,#22818));
#4333=EDGE_LOOP('',(#22819,#22820,#22821));
#4334=EDGE_LOOP('',(#22822,#22823,#22824,#22825));
#4335=EDGE_LOOP('',(#22826,#22827,#22828));
#4336=EDGE_LOOP('',(#22829,#22830,#22831,#22832));
#4337=EDGE_LOOP('',(#22833,#22834,#22835));
#4338=EDGE_LOOP('',(#22836,#22837,#22838,#22839));
#4339=EDGE_LOOP('',(#22840,#22841,#22842));
#4340=EDGE_LOOP('',(#22843,#22844,#22845,#22846));
#4341=EDGE_LOOP('',(#22847,#22848,#22849));
#4342=EDGE_LOOP('',(#22850,#22851,#22852,#22853));
#4343=EDGE_LOOP('',(#22854,#22855,#22856));
#4344=EDGE_LOOP('',(#22857,#22858,#22859,#22860));
#4345=EDGE_LOOP('',(#22861,#22862,#22863));
#4346=EDGE_LOOP('',(#22864,#22865,#22866,#22867));
#4347=EDGE_LOOP('',(#22868,#22869,#22870));
#4348=EDGE_LOOP('',(#22871,#22872,#22873,#22874));
#4349=EDGE_LOOP('',(#22875,#22876,#22877));
#4350=EDGE_LOOP('',(#22878,#22879,#22880,#22881));
#4351=EDGE_LOOP('',(#22882,#22883,#22884));
#4352=EDGE_LOOP('',(#22885,#22886,#22887,#22888));
#4353=EDGE_LOOP('',(#22889,#22890,#22891));
#4354=EDGE_LOOP('',(#22892,#22893,#22894,#22895));
#4355=EDGE_LOOP('',(#22896,#22897,#22898));
#4356=EDGE_LOOP('',(#22899,#22900,#22901,#22902));
#4357=EDGE_LOOP('',(#22903,#22904,#22905));
#4358=EDGE_LOOP('',(#22906,#22907,#22908,#22909));
#4359=EDGE_LOOP('',(#22910,#22911,#22912));
#4360=EDGE_LOOP('',(#22913,#22914,#22915,#22916));
#4361=EDGE_LOOP('',(#22917,#22918,#22919));
#4362=EDGE_LOOP('',(#22920,#22921,#22922,#22923));
#4363=EDGE_LOOP('',(#22924,#22925,#22926));
#4364=EDGE_LOOP('',(#22927,#22928,#22929,#22930));
#4365=EDGE_LOOP('',(#22931,#22932,#22933));
#4366=EDGE_LOOP('',(#22934,#22935,#22936,#22937));
#4367=EDGE_LOOP('',(#22938,#22939,#22940));
#4368=EDGE_LOOP('',(#22941,#22942,#22943,#22944));
#4369=EDGE_LOOP('',(#22945,#22946,#22947));
#4370=EDGE_LOOP('',(#22948,#22949,#22950,#22951));
#4371=EDGE_LOOP('',(#22952,#22953,#22954));
#4372=EDGE_LOOP('',(#22955,#22956,#22957,#22958));
#4373=EDGE_LOOP('',(#22959,#22960,#22961));
#4374=EDGE_LOOP('',(#22962,#22963,#22964,#22965));
#4375=EDGE_LOOP('',(#22966,#22967,#22968));
#4376=EDGE_LOOP('',(#22969,#22970,#22971,#22972));
#4377=EDGE_LOOP('',(#22973,#22974,#22975));
#4378=EDGE_LOOP('',(#22976,#22977,#22978,#22979));
#4379=EDGE_LOOP('',(#22980,#22981,#22982));
#4380=EDGE_LOOP('',(#22983,#22984,#22985,#22986));
#4381=EDGE_LOOP('',(#22987,#22988,#22989));
#4382=EDGE_LOOP('',(#22990,#22991,#22992,#22993));
#4383=EDGE_LOOP('',(#22994,#22995,#22996));
#4384=EDGE_LOOP('',(#22997,#22998,#22999,#23000));
#4385=EDGE_LOOP('',(#23001,#23002,#23003));
#4386=EDGE_LOOP('',(#23004,#23005,#23006,#23007));
#4387=EDGE_LOOP('',(#23008,#23009,#23010));
#4388=EDGE_LOOP('',(#23011,#23012,#23013,#23014));
#4389=EDGE_LOOP('',(#23015,#23016,#23017));
#4390=EDGE_LOOP('',(#23018,#23019,#23020,#23021));
#4391=EDGE_LOOP('',(#23022,#23023,#23024));
#4392=EDGE_LOOP('',(#23025,#23026,#23027,#23028));
#4393=EDGE_LOOP('',(#23029,#23030,#23031));
#4394=EDGE_LOOP('',(#23032,#23033,#23034,#23035));
#4395=EDGE_LOOP('',(#23036,#23037,#23038));
#4396=EDGE_LOOP('',(#23039,#23040,#23041,#23042));
#4397=EDGE_LOOP('',(#23043,#23044,#23045));
#4398=EDGE_LOOP('',(#23046,#23047,#23048,#23049));
#4399=EDGE_LOOP('',(#23050,#23051,#23052));
#4400=EDGE_LOOP('',(#23053,#23054,#23055,#23056));
#4401=EDGE_LOOP('',(#23057,#23058,#23059,#23060));
#4402=EDGE_LOOP('',(#23061,#23062,#23063,#23064));
#4403=EDGE_LOOP('',(#23065,#23066,#23067,#23068));
#4404=EDGE_LOOP('',(#23069,#23070,#23071,#23072));
#4405=EDGE_LOOP('',(#23073,#23074,#23075));
#4406=EDGE_LOOP('',(#23076,#23077,#23078,#23079));
#4407=EDGE_LOOP('',(#23080,#23081,#23082));
#4408=EDGE_LOOP('',(#23083,#23084,#23085,#23086));
#4409=EDGE_LOOP('',(#23087,#23088,#23089));
#4410=EDGE_LOOP('',(#23090,#23091,#23092,#23093));
#4411=EDGE_LOOP('',(#23094,#23095,#23096));
#4412=EDGE_LOOP('',(#23097,#23098,#23099,#23100));
#4413=EDGE_LOOP('',(#23101,#23102,#23103));
#4414=EDGE_LOOP('',(#23104,#23105,#23106,#23107));
#4415=EDGE_LOOP('',(#23108,#23109,#23110));
#4416=EDGE_LOOP('',(#23111,#23112,#23113,#23114));
#4417=EDGE_LOOP('',(#23115,#23116,#23117));
#4418=EDGE_LOOP('',(#23118,#23119,#23120,#23121));
#4419=EDGE_LOOP('',(#23122,#23123,#23124));
#4420=EDGE_LOOP('',(#23125,#23126,#23127,#23128));
#4421=EDGE_LOOP('',(#23129,#23130,#23131));
#4422=EDGE_LOOP('',(#23132,#23133,#23134,#23135));
#4423=EDGE_LOOP('',(#23136,#23137,#23138));
#4424=EDGE_LOOP('',(#23139,#23140,#23141,#23142));
#4425=EDGE_LOOP('',(#23143,#23144,#23145));
#4426=EDGE_LOOP('',(#23146,#23147,#23148,#23149));
#4427=EDGE_LOOP('',(#23150,#23151,#23152));
#4428=EDGE_LOOP('',(#23153,#23154,#23155,#23156));
#4429=EDGE_LOOP('',(#23157,#23158,#23159));
#4430=EDGE_LOOP('',(#23160,#23161,#23162,#23163));
#4431=EDGE_LOOP('',(#23164,#23165,#23166));
#4432=EDGE_LOOP('',(#23167,#23168,#23169,#23170));
#4433=EDGE_LOOP('',(#23171,#23172,#23173));
#4434=EDGE_LOOP('',(#23174,#23175,#23176,#23177));
#4435=EDGE_LOOP('',(#23178,#23179,#23180));
#4436=EDGE_LOOP('',(#23181,#23182,#23183,#23184));
#4437=EDGE_LOOP('',(#23185,#23186,#23187));
#4438=EDGE_LOOP('',(#23188,#23189,#23190,#23191));
#4439=EDGE_LOOP('',(#23192,#23193,#23194));
#4440=EDGE_LOOP('',(#23195,#23196,#23197,#23198));
#4441=EDGE_LOOP('',(#23199,#23200,#23201));
#4442=EDGE_LOOP('',(#23202,#23203,#23204,#23205));
#4443=EDGE_LOOP('',(#23206,#23207,#23208));
#4444=EDGE_LOOP('',(#23209,#23210,#23211,#23212));
#4445=EDGE_LOOP('',(#23213,#23214,#23215));
#4446=EDGE_LOOP('',(#23216,#23217,#23218,#23219));
#4447=EDGE_LOOP('',(#23220,#23221,#23222));
#4448=EDGE_LOOP('',(#23223,#23224,#23225,#23226));
#4449=EDGE_LOOP('',(#23227,#23228,#23229));
#4450=EDGE_LOOP('',(#23230,#23231,#23232,#23233));
#4451=EDGE_LOOP('',(#23234,#23235,#23236));
#4452=EDGE_LOOP('',(#23237,#23238,#23239,#23240));
#4453=EDGE_LOOP('',(#23241,#23242,#23243));
#4454=EDGE_LOOP('',(#23244,#23245,#23246,#23247));
#4455=EDGE_LOOP('',(#23248,#23249,#23250));
#4456=EDGE_LOOP('',(#23251,#23252,#23253,#23254));
#4457=EDGE_LOOP('',(#23255,#23256,#23257));
#4458=EDGE_LOOP('',(#23258,#23259,#23260,#23261));
#4459=EDGE_LOOP('',(#23262,#23263,#23264));
#4460=EDGE_LOOP('',(#23265,#23266,#23267,#23268));
#4461=EDGE_LOOP('',(#23269,#23270,#23271));
#4462=EDGE_LOOP('',(#23272,#23273,#23274,#23275));
#4463=EDGE_LOOP('',(#23276,#23277,#23278));
#4464=EDGE_LOOP('',(#23279,#23280,#23281,#23282));
#4465=EDGE_LOOP('',(#23283,#23284,#23285));
#4466=EDGE_LOOP('',(#23286,#23287,#23288,#23289));
#4467=EDGE_LOOP('',(#23290,#23291,#23292));
#4468=EDGE_LOOP('',(#23293,#23294,#23295,#23296));
#4469=EDGE_LOOP('',(#23297,#23298,#23299));
#4470=EDGE_LOOP('',(#23300,#23301,#23302,#23303));
#4471=EDGE_LOOP('',(#23304,#23305,#23306));
#4472=EDGE_LOOP('',(#23307,#23308,#23309,#23310));
#4473=EDGE_LOOP('',(#23311,#23312,#23313));
#4474=EDGE_LOOP('',(#23314,#23315,#23316,#23317));
#4475=EDGE_LOOP('',(#23318,#23319,#23320));
#4476=EDGE_LOOP('',(#23321,#23322,#23323,#23324));
#4477=EDGE_LOOP('',(#23325,#23326,#23327,#23328));
#4478=EDGE_LOOP('',(#23329,#23330,#23331,#23332));
#4479=EDGE_LOOP('',(#23333,#23334,#23335,#23336));
#4480=EDGE_LOOP('',(#23337,#23338,#23339,#23340));
#4481=EDGE_LOOP('',(#23341,#23342,#23343,#23344));
#4482=EDGE_LOOP('',(#23345,#23346,#23347,#23348,#23349,#23350));
#4483=EDGE_LOOP('',(#23351));
#4484=EDGE_LOOP('',(#23352,#23353,#23354,#23355,#23356,#23357));
#4485=EDGE_LOOP('',(#23358,#23359,#23360));
#4486=EDGE_LOOP('',(#23361,#23362,#23363,#23364,#23365,#23366));
#4487=EDGE_LOOP('',(#23367,#23368,#23369,#23370));
#4488=EDGE_LOOP('',(#23371));
#4489=EDGE_LOOP('',(#23372));
#4490=EDGE_LOOP('',(#23373,#23374,#23375,#23376,#23377,#23378,#23379,#23380,
#23381,#23382,#23383,#23384));
#4491=EDGE_LOOP('',(#23385,#23386,#23387,#23388));
#4492=EDGE_LOOP('',(#23389,#23390,#23391,#23392));
#4493=EDGE_LOOP('',(#23393,#23394,#23395,#23396));
#4494=EDGE_LOOP('',(#23397,#23398,#23399,#23400));
#4495=EDGE_LOOP('',(#23401,#23402,#23403,#23404));
#4496=EDGE_LOOP('',(#23405,#23406,#23407,#23408));
#4497=EDGE_LOOP('',(#23409,#23410,#23411,#23412));
#4498=EDGE_LOOP('',(#23413,#23414,#23415,#23416));
#4499=EDGE_LOOP('',(#23417,#23418,#23419,#23420));
#4500=EDGE_LOOP('',(#23421,#23422,#23423,#23424));
#4501=EDGE_LOOP('',(#23425,#23426,#23427,#23428));
#4502=EDGE_LOOP('',(#23429,#23430,#23431,#23432));
#4503=EDGE_LOOP('',(#23433,#23434,#23435,#23436));
#4504=EDGE_LOOP('',(#23437,#23438,#23439,#23440));
#4505=EDGE_LOOP('',(#23441,#23442,#23443,#23444));
#4506=EDGE_LOOP('',(#23445,#23446,#23447,#23448));
#4507=EDGE_LOOP('',(#23449,#23450,#23451,#23452));
#4508=EDGE_LOOP('',(#23453,#23454,#23455,#23456));
#4509=EDGE_LOOP('',(#23457,#23458,#23459,#23460));
#4510=EDGE_LOOP('',(#23461,#23462,#23463,#23464));
#4511=EDGE_LOOP('',(#23465,#23466,#23467,#23468));
#4512=EDGE_LOOP('',(#23469,#23470,#23471,#23472));
#4513=EDGE_LOOP('',(#23473,#23474,#23475,#23476));
#4514=EDGE_LOOP('',(#23477,#23478,#23479,#23480));
#4515=EDGE_LOOP('',(#23481,#23482,#23483,#23484));
#4516=EDGE_LOOP('',(#23485,#23486,#23487,#23488));
#4517=EDGE_LOOP('',(#23489,#23490,#23491,#23492));
#4518=EDGE_LOOP('',(#23493,#23494,#23495,#23496));
#4519=EDGE_LOOP('',(#23497,#23498,#23499,#23500));
#4520=EDGE_LOOP('',(#23501,#23502,#23503,#23504));
#4521=EDGE_LOOP('',(#23505,#23506,#23507,#23508));
#4522=EDGE_LOOP('',(#23509,#23510,#23511,#23512));
#4523=EDGE_LOOP('',(#23513,#23514,#23515,#23516));
#4524=EDGE_LOOP('',(#23517,#23518,#23519,#23520));
#4525=EDGE_LOOP('',(#23521,#23522,#23523,#23524));
#4526=EDGE_LOOP('',(#23525,#23526,#23527,#23528));
#4527=EDGE_LOOP('',(#23529));
#4528=EDGE_LOOP('',(#23530,#23531,#23532,#23533,#23534,#23535));
#4529=EDGE_LOOP('',(#23536));
#4530=EDGE_LOOP('',(#23537,#23538,#23539,#23540));
#4531=EDGE_LOOP('',(#23541,#23542,#23543,#23544));
#4532=EDGE_LOOP('',(#23545,#23546,#23547,#23548));
#4533=EDGE_LOOP('',(#23549));
#4534=LINE('',#33462,#7403);
#4535=LINE('',#33469,#7404);
#4536=LINE('',#33475,#7405);
#4537=LINE('',#33482,#7406);
#4538=LINE('',#33488,#7407);
#4539=LINE('',#33494,#7408);
#4540=LINE('',#33502,#7409);
#4541=LINE('',#33506,#7410);
#4542=LINE('',#33510,#7411);
#4543=LINE('',#33654,#7412);
#4544=LINE('',#33687,#7413);
#4545=LINE('',#33697,#7414);
#4546=LINE('',#33698,#7415);
#4547=LINE('',#33699,#7416);
#4548=LINE('',#33703,#7417);
#4549=LINE('',#33707,#7418);
#4550=LINE('',#33711,#7419);
#4551=LINE('',#33715,#7420);
#4552=LINE('',#33719,#7421);
#4553=LINE('',#33724,#7422);
#4554=LINE('',#33726,#7423);
#4555=LINE('',#33728,#7424);
#4556=LINE('',#33732,#7425);
#4557=LINE('',#33734,#7426);
#4558=LINE('',#33736,#7427);
#4559=LINE('',#33742,#7428);
#4560=LINE('',#33746,#7429);
#4561=LINE('',#33750,#7430);
#4562=LINE('',#33756,#7431);
#4563=LINE('',#33758,#7432);
#4564=LINE('',#33760,#7433);
#4565=LINE('',#33762,#7434);
#4566=LINE('',#33764,#7435);
#4567=LINE('',#33767,#7436);
#4568=LINE('',#33772,#7437);
#4569=LINE('',#33777,#7438);
#4570=LINE('',#33792,#7439);
#4571=LINE('',#33797,#7440);
#4572=LINE('',#33802,#7441);
#4573=LINE('',#33868,#7442);
#4574=LINE('',#33869,#7443);
#4575=LINE('',#33983,#7444);
#4576=LINE('',#33993,#7445);
#4577=LINE('',#33994,#7446);
#4578=LINE('',#33997,#7447);
#4579=LINE('',#34014,#7448);
#4580=LINE('',#34015,#7449);
#4581=LINE('',#34018,#7450);
#4582=LINE('',#34023,#7451);
#4583=LINE('',#34026,#7452);
#4584=LINE('',#34031,#7453);
#4585=LINE('',#34042,#7454);
#4586=LINE('',#34050,#7455);
#4587=LINE('',#34055,#7456);
#4588=LINE('',#34069,#7457);
#4589=LINE('',#34090,#7458);
#4590=LINE('',#34098,#7459);
#4591=LINE('',#34103,#7460);
#4592=LINE('',#34126,#7461);
#4593=LINE('',#34143,#7462);
#4594=LINE('',#34159,#7463);
#4595=LINE('',#34163,#7464);
#4596=LINE('',#34169,#7465);
#4597=LINE('',#34173,#7466);
#4598=LINE('',#34177,#7467);
#4599=LINE('',#34180,#7468);
#4600=LINE('',#34189,#7469);
#4601=LINE('',#34193,#7470);
#4602=LINE('',#34204,#7471);
#4603=LINE('',#34206,#7472);
#4604=LINE('',#34208,#7473);
#4605=LINE('',#34211,#7474);
#4606=LINE('',#34216,#7475);
#4607=LINE('',#34219,#7476);
#4608=LINE('',#34224,#7477);
#4609=LINE('',#34397,#7478);
#4610=LINE('',#34407,#7479);
#4611=LINE('',#34408,#7480);
#4612=LINE('',#34409,#7481);
#4613=LINE('',#34412,#7482);
#4614=LINE('',#34477,#7483);
#4615=LINE('',#34478,#7484);
#4616=LINE('',#34588,#7485);
#4617=LINE('',#34597,#7486);
#4618=LINE('',#34598,#7487);
#4619=LINE('',#34601,#7488);
#4620=LINE('',#34618,#7489);
#4621=LINE('',#34619,#7490);
#4622=LINE('',#34621,#7491);
#4623=LINE('',#34623,#7492);
#4624=LINE('',#34627,#7493);
#4625=LINE('',#34629,#7494);
#4626=LINE('',#34631,#7495);
#4627=LINE('',#34632,#7496);
#4628=LINE('',#34635,#7497);
#4629=LINE('',#34640,#7498);
#4630=LINE('',#34641,#7499);
#4631=LINE('',#34645,#7500);
#4632=LINE('',#34651,#7501);
#4633=LINE('',#34652,#7502);
#4634=LINE('',#34653,#7503);
#4635=LINE('',#34655,#7504);
#4636=LINE('',#34689,#7505);
#4637=LINE('',#34692,#7506);
#4638=LINE('',#34749,#7507);
#4639=LINE('',#34751,#7508);
#4640=LINE('',#34754,#7509);
#4641=LINE('',#34757,#7510);
#4642=LINE('',#34760,#7511);
#4643=LINE('',#34761,#7512);
#4644=LINE('',#34764,#7513);
#4645=LINE('',#34822,#7514);
#4646=LINE('',#34824,#7515);
#4647=LINE('',#34827,#7516);
#4648=LINE('',#34830,#7517);
#4649=LINE('',#34833,#7518);
#4650=LINE('',#34834,#7519);
#4651=LINE('',#34837,#7520);
#4652=LINE('',#34888,#7521);
#4653=LINE('',#34923,#7522);
#4654=LINE('',#34926,#7523);
#4655=LINE('',#34930,#7524);
#4656=LINE('',#34987,#7525);
#4657=LINE('',#34993,#7526);
#4658=LINE('',#34996,#7527);
#4659=LINE('',#34997,#7528);
#4660=LINE('',#35000,#7529);
#4661=LINE('',#35004,#7530);
#4662=LINE('',#35005,#7531);
#4663=LINE('',#35008,#7532);
#4664=LINE('',#35012,#7533);
#4665=LINE('',#35013,#7534);
#4666=LINE('',#35016,#7535);
#4667=LINE('',#35020,#7536);
#4668=LINE('',#35026,#7537);
#4669=LINE('',#35035,#7538);
#4670=LINE('',#35043,#7539);
#4671=LINE('',#35049,#7540);
#4672=LINE('',#35055,#7541);
#4673=LINE('',#35058,#7542);
#4674=LINE('',#35061,#7543);
#4675=LINE('',#35064,#7544);
#4676=LINE('',#35065,#7545);
#4677=LINE('',#35068,#7546);
#4678=LINE('',#35072,#7547);
#4679=LINE('',#35073,#7548);
#4680=LINE('',#35076,#7549);
#4681=LINE('',#35079,#7550);
#4682=LINE('',#35081,#7551);
#4683=LINE('',#35083,#7552);
#4684=LINE('',#35085,#7553);
#4685=LINE('',#35119,#7554);
#4686=LINE('',#35125,#7555);
#4687=LINE('',#35128,#7556);
#4688=LINE('',#35129,#7557);
#4689=LINE('',#35146,#7558);
#4690=LINE('',#35152,#7559);
#4691=LINE('',#35184,#7560);
#4692=LINE('',#35195,#7561);
#4693=LINE('',#35197,#7562);
#4694=LINE('',#35210,#7563);
#4695=LINE('',#35219,#7564);
#4696=LINE('',#35224,#7565);
#4697=LINE('',#35227,#7566);
#4698=LINE('',#35230,#7567);
#4699=LINE('',#35231,#7568);
#4700=LINE('',#35236,#7569);
#4701=LINE('',#35245,#7570);
#4702=LINE('',#35250,#7571);
#4703=LINE('',#35253,#7572);
#4704=LINE('',#35256,#7573);
#4705=LINE('',#35257,#7574);
#4706=LINE('',#35260,#7575);
#4707=LINE('',#35263,#7576);
#4708=LINE('',#35266,#7577);
#4709=LINE('',#35269,#7578);
#4710=LINE('',#35273,#7579);
#4711=LINE('',#35278,#7580);
#4712=LINE('',#35288,#7581);
#4713=LINE('',#35294,#7582);
#4714=LINE('',#35296,#7583);
#4715=LINE('',#35301,#7584);
#4716=LINE('',#35305,#7585);
#4717=LINE('',#35307,#7586);
#4718=LINE('',#35309,#7587);
#4719=LINE('',#35311,#7588);
#4720=LINE('',#35313,#7589);
#4721=LINE('',#35317,#7590);
#4722=LINE('',#35324,#7591);
#4723=LINE('',#35328,#7592);
#4724=LINE('',#35337,#7593);
#4725=LINE('',#35341,#7594);
#4726=LINE('',#35351,#7595);
#4727=LINE('',#35354,#7596);
#4728=LINE('',#35365,#7597);
#4729=LINE('',#35366,#7598);
#4730=LINE('',#35377,#7599);
#4731=LINE('',#35378,#7600);
#4732=LINE('',#35389,#7601);
#4733=LINE('',#35390,#7602);
#4734=LINE('',#35396,#7603);
#4735=LINE('',#35399,#7604);
#4736=LINE('',#35402,#7605);
#4737=LINE('',#35403,#7606);
#4738=LINE('',#35406,#7607);
#4739=LINE('',#35410,#7608);
#4740=LINE('',#35411,#7609);
#4741=LINE('',#35436,#7610);
#4742=LINE('',#35447,#7611);
#4743=LINE('',#35448,#7612);
#4744=LINE('',#35458,#7613);
#4745=LINE('',#35459,#7614);
#4746=LINE('',#35467,#7615);
#4747=LINE('',#35471,#7616);
#4748=LINE('',#35472,#7617);
#4749=LINE('',#35474,#7618);
#4750=LINE('',#35495,#7619);
#4751=LINE('',#35500,#7620);
#4752=LINE('',#35505,#7621);
#4753=LINE('',#35510,#7622);
#4754=LINE('',#35514,#7623);
#4755=LINE('',#35516,#7624);
#4756=LINE('',#35518,#7625);
#4757=LINE('',#35520,#7626);
#4758=LINE('',#35525,#7627);
#4759=LINE('',#35583,#7628);
#4760=LINE('',#35585,#7629);
#4761=LINE('',#35616,#7630);
#4762=LINE('',#35617,#7631);
#4763=LINE('',#35622,#7632);
#4764=LINE('',#35626,#7633);
#4765=LINE('',#35656,#7634);
#4766=LINE('',#35663,#7635);
#4767=LINE('',#35670,#7636);
#4768=LINE('',#35675,#7637);
#4769=LINE('',#35677,#7638);
#4770=LINE('',#35679,#7639);
#4771=LINE('',#35680,#7640);
#4772=LINE('',#35684,#7641);
#4773=LINE('',#35690,#7642);
#4774=LINE('',#35691,#7643);
#4775=LINE('',#35692,#7644);
#4776=LINE('',#35698,#7645);
#4777=LINE('',#35701,#7646);
#4778=LINE('',#35704,#7647);
#4779=LINE('',#35705,#7648);
#4780=LINE('',#35711,#7649);
#4781=LINE('',#35715,#7650);
#4782=LINE('',#35719,#7651);
#4783=LINE('',#35722,#7652);
#4784=LINE('',#35738,#7653);
#4785=LINE('',#35740,#7654);
#4786=LINE('',#35742,#7655);
#4787=LINE('',#35743,#7656);
#4788=LINE('',#35747,#7657);
#4789=LINE('',#35753,#7658);
#4790=LINE('',#35754,#7659);
#4791=LINE('',#35755,#7660);
#4792=LINE('',#35761,#7661);
#4793=LINE('',#35764,#7662);
#4794=LINE('',#35767,#7663);
#4795=LINE('',#35768,#7664);
#4796=LINE('',#35777,#7665);
#4797=LINE('',#35786,#7666);
#4798=LINE('',#35796,#7667);
#4799=LINE('',#35798,#7668);
#4800=LINE('',#35800,#7669);
#4801=LINE('',#35802,#7670);
#4802=LINE('',#35803,#7671);
#4803=LINE('',#35806,#7672);
#4804=LINE('',#35810,#7673);
#4805=LINE('',#35815,#7674);
#4806=LINE('',#35824,#7675);
#4807=LINE('',#35835,#7676);
#4808=LINE('',#35845,#7677);
#4809=LINE('',#35847,#7678);
#4810=LINE('',#35849,#7679);
#4811=LINE('',#35851,#7680);
#4812=LINE('',#35852,#7681);
#4813=LINE('',#35855,#7682);
#4814=LINE('',#35859,#7683);
#4815=LINE('',#35866,#7684);
#4816=LINE('',#35870,#7685);
#4817=LINE('',#35873,#7686);
#4818=LINE('',#35876,#7687);
#4819=LINE('',#35877,#7688);
#4820=LINE('',#35880,#7689);
#4821=LINE('',#35884,#7690);
#4822=LINE('',#35885,#7691);
#4823=LINE('',#35888,#7692);
#4824=LINE('',#35892,#7693);
#4825=LINE('',#35893,#7694);
#4826=LINE('',#35896,#7695);
#4827=LINE('',#35899,#7696);
#4828=LINE('',#35902,#7697);
#4829=LINE('',#35904,#7698);
#4830=LINE('',#35905,#7699);
#4831=LINE('',#35908,#7700);
#4832=LINE('',#35912,#7701);
#4833=LINE('',#35913,#7702);
#4834=LINE('',#35916,#7703);
#4835=LINE('',#35919,#7704);
#4836=LINE('',#35920,#7705);
#4837=LINE('',#35923,#7706);
#4838=LINE('',#35927,#7707);
#4839=LINE('',#35928,#7708);
#4840=LINE('',#35930,#7709);
#4841=LINE('',#35934,#7710);
#4842=LINE('',#35935,#7711);
#4843=LINE('',#35939,#7712);
#4844=LINE('',#35945,#7713);
#4845=LINE('',#35946,#7714);
#4846=LINE('',#35947,#7715);
#4847=LINE('',#35953,#7716);
#4848=LINE('',#35957,#7717);
#4849=LINE('',#35958,#7718);
#4850=LINE('',#35963,#7719);
#4851=LINE('',#35967,#7720);
#4852=LINE('',#35968,#7721);
#4853=LINE('',#35976,#7722);
#4854=LINE('',#35979,#7723);
#4855=LINE('',#35982,#7724);
#4856=LINE('',#35985,#7725);
#4857=LINE('',#35988,#7726);
#4858=LINE('',#35992,#7727);
#4859=LINE('',#35997,#7728);
#4860=LINE('',#36003,#7729);
#4861=LINE('',#36007,#7730);
#4862=LINE('',#36011,#7731);
#4863=LINE('',#36015,#7732);
#4864=LINE('',#36021,#7733);
#4865=LINE('',#36023,#7734);
#4866=LINE('',#36025,#7735);
#4867=LINE('',#36031,#7736);
#4868=LINE('',#36033,#7737);
#4869=LINE('',#36035,#7738);
#4870=LINE('',#36037,#7739);
#4871=LINE('',#36039,#7740);
#4872=LINE('',#36040,#7741);
#4873=LINE('',#36043,#7742);
#4874=LINE('',#36045,#7743);
#4875=LINE('',#36047,#7744);
#4876=LINE('',#36049,#7745);
#4877=LINE('',#36051,#7746);
#4878=LINE('',#36053,#7747);
#4879=LINE('',#36055,#7748);
#4880=LINE('',#36057,#7749);
#4881=LINE('',#36059,#7750);
#4882=LINE('',#36061,#7751);
#4883=LINE('',#36063,#7752);
#4884=LINE('',#36065,#7753);
#4885=LINE('',#36067,#7754);
#4886=LINE('',#36069,#7755);
#4887=LINE('',#36071,#7756);
#4888=LINE('',#36073,#7757);
#4889=LINE('',#36075,#7758);
#4890=LINE('',#36077,#7759);
#4891=LINE('',#36079,#7760);
#4892=LINE('',#36081,#7761);
#4893=LINE('',#36083,#7762);
#4894=LINE('',#36085,#7763);
#4895=LINE('',#36087,#7764);
#4896=LINE('',#36089,#7765);
#4897=LINE('',#36091,#7766);
#4898=LINE('',#36093,#7767);
#4899=LINE('',#36095,#7768);
#4900=LINE('',#36097,#7769);
#4901=LINE('',#36099,#7770);
#4902=LINE('',#36101,#7771);
#4903=LINE('',#36103,#7772);
#4904=LINE('',#36105,#7773);
#4905=LINE('',#36107,#7774);
#4906=LINE('',#36109,#7775);
#4907=LINE('',#36111,#7776);
#4908=LINE('',#36113,#7777);
#4909=LINE('',#36115,#7778);
#4910=LINE('',#36117,#7779);
#4911=LINE('',#36119,#7780);
#4912=LINE('',#36121,#7781);
#4913=LINE('',#36123,#7782);
#4914=LINE('',#36125,#7783);
#4915=LINE('',#36127,#7784);
#4916=LINE('',#36129,#7785);
#4917=LINE('',#36131,#7786);
#4918=LINE('',#36133,#7787);
#4919=LINE('',#36135,#7788);
#4920=LINE('',#36137,#7789);
#4921=LINE('',#36139,#7790);
#4922=LINE('',#36141,#7791);
#4923=LINE('',#36143,#7792);
#4924=LINE('',#36145,#7793);
#4925=LINE('',#36147,#7794);
#4926=LINE('',#36149,#7795);
#4927=LINE('',#36151,#7796);
#4928=LINE('',#36153,#7797);
#4929=LINE('',#36155,#7798);
#4930=LINE('',#36157,#7799);
#4931=LINE('',#36159,#7800);
#4932=LINE('',#36161,#7801);
#4933=LINE('',#36163,#7802);
#4934=LINE('',#36165,#7803);
#4935=LINE('',#36167,#7804);
#4936=LINE('',#36169,#7805);
#4937=LINE('',#36171,#7806);
#4938=LINE('',#36173,#7807);
#4939=LINE('',#36175,#7808);
#4940=LINE('',#36177,#7809);
#4941=LINE('',#36179,#7810);
#4942=LINE('',#36181,#7811);
#4943=LINE('',#36183,#7812);
#4944=LINE('',#36185,#7813);
#4945=LINE('',#36187,#7814);
#4946=LINE('',#36189,#7815);
#4947=LINE('',#36191,#7816);
#4948=LINE('',#36193,#7817);
#4949=LINE('',#36195,#7818);
#4950=LINE('',#36197,#7819);
#4951=LINE('',#36199,#7820);
#4952=LINE('',#36201,#7821);
#4953=LINE('',#36203,#7822);
#4954=LINE('',#36205,#7823);
#4955=LINE('',#36207,#7824);
#4956=LINE('',#36209,#7825);
#4957=LINE('',#36211,#7826);
#4958=LINE('',#36213,#7827);
#4959=LINE('',#36215,#7828);
#4960=LINE('',#36217,#7829);
#4961=LINE('',#36219,#7830);
#4962=LINE('',#36221,#7831);
#4963=LINE('',#36223,#7832);
#4964=LINE('',#36225,#7833);
#4965=LINE('',#36227,#7834);
#4966=LINE('',#36229,#7835);
#4967=LINE('',#36231,#7836);
#4968=LINE('',#36233,#7837);
#4969=LINE('',#36235,#7838);
#4970=LINE('',#36237,#7839);
#4971=LINE('',#36239,#7840);
#4972=LINE('',#36241,#7841);
#4973=LINE('',#36243,#7842);
#4974=LINE('',#36245,#7843);
#4975=LINE('',#36247,#7844);
#4976=LINE('',#36249,#7845);
#4977=LINE('',#36251,#7846);
#4978=LINE('',#36253,#7847);
#4979=LINE('',#36255,#7848);
#4980=LINE('',#36257,#7849);
#4981=LINE('',#36259,#7850);
#4982=LINE('',#36261,#7851);
#4983=LINE('',#36263,#7852);
#4984=LINE('',#36265,#7853);
#4985=LINE('',#36267,#7854);
#4986=LINE('',#36269,#7855);
#4987=LINE('',#36271,#7856);
#4988=LINE('',#36273,#7857);
#4989=LINE('',#36275,#7858);
#4990=LINE('',#36277,#7859);
#4991=LINE('',#36279,#7860);
#4992=LINE('',#36281,#7861);
#4993=LINE('',#36283,#7862);
#4994=LINE('',#36285,#7863);
#4995=LINE('',#36287,#7864);
#4996=LINE('',#36289,#7865);
#4997=LINE('',#36291,#7866);
#4998=LINE('',#36293,#7867);
#4999=LINE('',#36295,#7868);
#5000=LINE('',#36297,#7869);
#5001=LINE('',#36299,#7870);
#5002=LINE('',#36301,#7871);
#5003=LINE('',#36303,#7872);
#5004=LINE('',#36305,#7873);
#5005=LINE('',#36307,#7874);
#5006=LINE('',#36309,#7875);
#5007=LINE('',#36311,#7876);
#5008=LINE('',#36313,#7877);
#5009=LINE('',#36315,#7878);
#5010=LINE('',#36317,#7879);
#5011=LINE('',#36319,#7880);
#5012=LINE('',#36321,#7881);
#5013=LINE('',#36323,#7882);
#5014=LINE('',#36325,#7883);
#5015=LINE('',#36327,#7884);
#5016=LINE('',#36329,#7885);
#5017=LINE('',#36331,#7886);
#5018=LINE('',#36333,#7887);
#5019=LINE('',#36335,#7888);
#5020=LINE('',#36337,#7889);
#5021=LINE('',#36339,#7890);
#5022=LINE('',#36341,#7891);
#5023=LINE('',#36343,#7892);
#5024=LINE('',#36345,#7893);
#5025=LINE('',#36347,#7894);
#5026=LINE('',#36349,#7895);
#5027=LINE('',#36351,#7896);
#5028=LINE('',#36353,#7897);
#5029=LINE('',#36355,#7898);
#5030=LINE('',#36357,#7899);
#5031=LINE('',#36359,#7900);
#5032=LINE('',#36361,#7901);
#5033=LINE('',#36363,#7902);
#5034=LINE('',#36365,#7903);
#5035=LINE('',#36367,#7904);
#5036=LINE('',#36369,#7905);
#5037=LINE('',#36371,#7906);
#5038=LINE('',#36373,#7907);
#5039=LINE('',#36375,#7908);
#5040=LINE('',#36377,#7909);
#5041=LINE('',#36379,#7910);
#5042=LINE('',#36381,#7911);
#5043=LINE('',#36383,#7912);
#5044=LINE('',#36385,#7913);
#5045=LINE('',#36387,#7914);
#5046=LINE('',#36389,#7915);
#5047=LINE('',#36391,#7916);
#5048=LINE('',#36393,#7917);
#5049=LINE('',#36395,#7918);
#5050=LINE('',#36397,#7919);
#5051=LINE('',#36399,#7920);
#5052=LINE('',#36401,#7921);
#5053=LINE('',#36403,#7922);
#5054=LINE('',#36405,#7923);
#5055=LINE('',#36407,#7924);
#5056=LINE('',#36409,#7925);
#5057=LINE('',#36411,#7926);
#5058=LINE('',#36413,#7927);
#5059=LINE('',#36415,#7928);
#5060=LINE('',#36417,#7929);
#5061=LINE('',#36419,#7930);
#5062=LINE('',#36421,#7931);
#5063=LINE('',#36423,#7932);
#5064=LINE('',#36425,#7933);
#5065=LINE('',#36427,#7934);
#5066=LINE('',#36429,#7935);
#5067=LINE('',#36431,#7936);
#5068=LINE('',#36433,#7937);
#5069=LINE('',#36435,#7938);
#5070=LINE('',#36437,#7939);
#5071=LINE('',#36439,#7940);
#5072=LINE('',#36441,#7941);
#5073=LINE('',#36443,#7942);
#5074=LINE('',#36445,#7943);
#5075=LINE('',#36447,#7944);
#5076=LINE('',#36449,#7945);
#5077=LINE('',#36451,#7946);
#5078=LINE('',#36453,#7947);
#5079=LINE('',#36455,#7948);
#5080=LINE('',#36457,#7949);
#5081=LINE('',#36459,#7950);
#5082=LINE('',#36461,#7951);
#5083=LINE('',#36463,#7952);
#5084=LINE('',#36465,#7953);
#5085=LINE('',#36467,#7954);
#5086=LINE('',#36469,#7955);
#5087=LINE('',#36471,#7956);
#5088=LINE('',#36473,#7957);
#5089=LINE('',#36475,#7958);
#5090=LINE('',#36477,#7959);
#5091=LINE('',#36479,#7960);
#5092=LINE('',#36481,#7961);
#5093=LINE('',#36483,#7962);
#5094=LINE('',#36485,#7963);
#5095=LINE('',#36487,#7964);
#5096=LINE('',#36489,#7965);
#5097=LINE('',#36491,#7966);
#5098=LINE('',#36493,#7967);
#5099=LINE('',#36495,#7968);
#5100=LINE('',#36497,#7969);
#5101=LINE('',#36499,#7970);
#5102=LINE('',#36501,#7971);
#5103=LINE('',#36503,#7972);
#5104=LINE('',#36505,#7973);
#5105=LINE('',#36507,#7974);
#5106=LINE('',#36509,#7975);
#5107=LINE('',#36511,#7976);
#5108=LINE('',#36513,#7977);
#5109=LINE('',#36515,#7978);
#5110=LINE('',#36517,#7979);
#5111=LINE('',#36518,#7980);
#5112=LINE('',#36523,#7981);
#5113=LINE('',#36525,#7982);
#5114=LINE('',#36527,#7983);
#5115=LINE('',#36528,#7984);
#5116=LINE('',#36531,#7985);
#5117=LINE('',#36532,#7986);
#5118=LINE('',#36535,#7987);
#5119=LINE('',#36537,#7988);
#5120=LINE('',#36539,#7989);
#5121=LINE('',#36541,#7990);
#5122=LINE('',#36542,#7991);
#5123=LINE('',#36545,#7992);
#5124=LINE('',#36547,#7993);
#5125=LINE('',#36549,#7994);
#5126=LINE('',#36550,#7995);
#5127=LINE('',#36553,#7996);
#5128=LINE('',#36554,#7997);
#5129=LINE('',#36557,#7998);
#5130=LINE('',#36559,#7999);
#5131=LINE('',#36561,#8000);
#5132=LINE('',#36563,#8001);
#5133=LINE('',#36564,#8002);
#5134=LINE('',#36567,#8003);
#5135=LINE('',#36569,#8004);
#5136=LINE('',#36571,#8005);
#5137=LINE('',#36572,#8006);
#5138=LINE('',#36575,#8007);
#5139=LINE('',#36576,#8008);
#5140=LINE('',#36579,#8009);
#5141=LINE('',#36581,#8010);
#5142=LINE('',#36583,#8011);
#5143=LINE('',#36585,#8012);
#5144=LINE('',#36586,#8013);
#5145=LINE('',#36589,#8014);
#5146=LINE('',#36591,#8015);
#5147=LINE('',#36593,#8016);
#5148=LINE('',#36594,#8017);
#5149=LINE('',#36597,#8018);
#5150=LINE('',#36598,#8019);
#5151=LINE('',#36601,#8020);
#5152=LINE('',#36603,#8021);
#5153=LINE('',#36605,#8022);
#5154=LINE('',#36607,#8023);
#5155=LINE('',#36608,#8024);
#5156=LINE('',#36611,#8025);
#5157=LINE('',#36613,#8026);
#5158=LINE('',#36615,#8027);
#5159=LINE('',#36616,#8028);
#5160=LINE('',#36619,#8029);
#5161=LINE('',#36620,#8030);
#5162=LINE('',#36623,#8031);
#5163=LINE('',#36625,#8032);
#5164=LINE('',#36627,#8033);
#5165=LINE('',#36629,#8034);
#5166=LINE('',#36630,#8035);
#5167=LINE('',#36633,#8036);
#5168=LINE('',#36635,#8037);
#5169=LINE('',#36637,#8038);
#5170=LINE('',#36638,#8039);
#5171=LINE('',#36641,#8040);
#5172=LINE('',#36642,#8041);
#5173=LINE('',#36645,#8042);
#5174=LINE('',#36647,#8043);
#5175=LINE('',#36649,#8044);
#5176=LINE('',#36651,#8045);
#5177=LINE('',#36652,#8046);
#5178=LINE('',#36655,#8047);
#5179=LINE('',#36657,#8048);
#5180=LINE('',#36659,#8049);
#5181=LINE('',#36660,#8050);
#5182=LINE('',#36663,#8051);
#5183=LINE('',#36664,#8052);
#5184=LINE('',#36667,#8053);
#5185=LINE('',#36669,#8054);
#5186=LINE('',#36671,#8055);
#5187=LINE('',#36673,#8056);
#5188=LINE('',#36674,#8057);
#5189=LINE('',#36677,#8058);
#5190=LINE('',#36679,#8059);
#5191=LINE('',#36681,#8060);
#5192=LINE('',#36682,#8061);
#5193=LINE('',#36685,#8062);
#5194=LINE('',#36686,#8063);
#5195=LINE('',#36689,#8064);
#5196=LINE('',#36691,#8065);
#5197=LINE('',#36693,#8066);
#5198=LINE('',#36695,#8067);
#5199=LINE('',#36696,#8068);
#5200=LINE('',#36699,#8069);
#5201=LINE('',#36701,#8070);
#5202=LINE('',#36703,#8071);
#5203=LINE('',#36704,#8072);
#5204=LINE('',#36707,#8073);
#5205=LINE('',#36708,#8074);
#5206=LINE('',#36711,#8075);
#5207=LINE('',#36713,#8076);
#5208=LINE('',#36715,#8077);
#5209=LINE('',#36717,#8078);
#5210=LINE('',#36718,#8079);
#5211=LINE('',#36721,#8080);
#5212=LINE('',#36723,#8081);
#5213=LINE('',#36725,#8082);
#5214=LINE('',#36726,#8083);
#5215=LINE('',#36729,#8084);
#5216=LINE('',#36730,#8085);
#5217=LINE('',#36733,#8086);
#5218=LINE('',#36735,#8087);
#5219=LINE('',#36737,#8088);
#5220=LINE('',#36739,#8089);
#5221=LINE('',#36740,#8090);
#5222=LINE('',#36743,#8091);
#5223=LINE('',#36745,#8092);
#5224=LINE('',#36747,#8093);
#5225=LINE('',#36748,#8094);
#5226=LINE('',#36751,#8095);
#5227=LINE('',#36752,#8096);
#5228=LINE('',#36755,#8097);
#5229=LINE('',#36757,#8098);
#5230=LINE('',#36759,#8099);
#5231=LINE('',#36761,#8100);
#5232=LINE('',#36762,#8101);
#5233=LINE('',#36765,#8102);
#5234=LINE('',#36767,#8103);
#5235=LINE('',#36769,#8104);
#5236=LINE('',#36770,#8105);
#5237=LINE('',#36773,#8106);
#5238=LINE('',#36774,#8107);
#5239=LINE('',#36778,#8108);
#5240=LINE('',#36780,#8109);
#5241=LINE('',#36781,#8110);
#5242=LINE('',#36783,#8111);
#5243=LINE('',#36784,#8112);
#5244=LINE('',#36787,#8113);
#5245=LINE('',#36789,#8114);
#5246=LINE('',#36790,#8115);
#5247=LINE('',#36793,#8116);
#5248=LINE('',#36794,#8117);
#5249=LINE('',#36798,#8118);
#5250=LINE('',#36800,#8119);
#5251=LINE('',#36801,#8120);
#5252=LINE('',#36803,#8121);
#5253=LINE('',#36804,#8122);
#5254=LINE('',#36807,#8123);
#5255=LINE('',#36809,#8124);
#5256=LINE('',#36810,#8125);
#5257=LINE('',#36813,#8126);
#5258=LINE('',#36814,#8127);
#5259=LINE('',#36818,#8128);
#5260=LINE('',#36820,#8129);
#5261=LINE('',#36821,#8130);
#5262=LINE('',#36823,#8131);
#5263=LINE('',#36824,#8132);
#5264=LINE('',#36827,#8133);
#5265=LINE('',#36829,#8134);
#5266=LINE('',#36830,#8135);
#5267=LINE('',#36833,#8136);
#5268=LINE('',#36834,#8137);
#5269=LINE('',#36838,#8138);
#5270=LINE('',#36840,#8139);
#5271=LINE('',#36841,#8140);
#5272=LINE('',#36843,#8141);
#5273=LINE('',#36844,#8142);
#5274=LINE('',#36847,#8143);
#5275=LINE('',#36849,#8144);
#5276=LINE('',#36850,#8145);
#5277=LINE('',#36853,#8146);
#5278=LINE('',#36854,#8147);
#5279=LINE('',#36858,#8148);
#5280=LINE('',#36860,#8149);
#5281=LINE('',#36861,#8150);
#5282=LINE('',#36863,#8151);
#5283=LINE('',#36864,#8152);
#5284=LINE('',#36867,#8153);
#5285=LINE('',#36869,#8154);
#5286=LINE('',#36870,#8155);
#5287=LINE('',#36873,#8156);
#5288=LINE('',#36874,#8157);
#5289=LINE('',#36878,#8158);
#5290=LINE('',#36880,#8159);
#5291=LINE('',#36881,#8160);
#5292=LINE('',#36883,#8161);
#5293=LINE('',#36884,#8162);
#5294=LINE('',#36887,#8163);
#5295=LINE('',#36889,#8164);
#5296=LINE('',#36890,#8165);
#5297=LINE('',#36893,#8166);
#5298=LINE('',#36894,#8167);
#5299=LINE('',#36898,#8168);
#5300=LINE('',#36900,#8169);
#5301=LINE('',#36901,#8170);
#5302=LINE('',#36903,#8171);
#5303=LINE('',#36904,#8172);
#5304=LINE('',#36907,#8173);
#5305=LINE('',#36909,#8174);
#5306=LINE('',#36910,#8175);
#5307=LINE('',#36913,#8176);
#5308=LINE('',#36914,#8177);
#5309=LINE('',#36918,#8178);
#5310=LINE('',#36920,#8179);
#5311=LINE('',#36921,#8180);
#5312=LINE('',#36923,#8181);
#5313=LINE('',#36924,#8182);
#5314=LINE('',#36927,#8183);
#5315=LINE('',#36929,#8184);
#5316=LINE('',#36930,#8185);
#5317=LINE('',#36933,#8186);
#5318=LINE('',#36934,#8187);
#5319=LINE('',#36938,#8188);
#5320=LINE('',#36940,#8189);
#5321=LINE('',#36941,#8190);
#5322=LINE('',#36943,#8191);
#5323=LINE('',#36944,#8192);
#5324=LINE('',#36947,#8193);
#5325=LINE('',#36949,#8194);
#5326=LINE('',#36950,#8195);
#5327=LINE('',#36953,#8196);
#5328=LINE('',#36954,#8197);
#5329=LINE('',#36958,#8198);
#5330=LINE('',#36960,#8199);
#5331=LINE('',#36961,#8200);
#5332=LINE('',#36963,#8201);
#5333=LINE('',#36964,#8202);
#5334=LINE('',#36967,#8203);
#5335=LINE('',#36969,#8204);
#5336=LINE('',#36970,#8205);
#5337=LINE('',#36973,#8206);
#5338=LINE('',#36974,#8207);
#5339=LINE('',#36978,#8208);
#5340=LINE('',#36980,#8209);
#5341=LINE('',#36981,#8210);
#5342=LINE('',#36983,#8211);
#5343=LINE('',#36984,#8212);
#5344=LINE('',#36987,#8213);
#5345=LINE('',#36989,#8214);
#5346=LINE('',#36990,#8215);
#5347=LINE('',#36993,#8216);
#5348=LINE('',#36994,#8217);
#5349=LINE('',#36998,#8218);
#5350=LINE('',#37000,#8219);
#5351=LINE('',#37001,#8220);
#5352=LINE('',#37003,#8221);
#5353=LINE('',#37004,#8222);
#5354=LINE('',#37007,#8223);
#5355=LINE('',#37009,#8224);
#5356=LINE('',#37010,#8225);
#5357=LINE('',#37013,#8226);
#5358=LINE('',#37014,#8227);
#5359=LINE('',#37017,#8228);
#5360=LINE('',#37019,#8229);
#5361=LINE('',#37021,#8230);
#5362=LINE('',#37022,#8231);
#5363=LINE('',#37025,#8232);
#5364=LINE('',#37027,#8233);
#5365=LINE('',#37029,#8234);
#5366=LINE('',#37031,#8235);
#5367=LINE('',#37033,#8236);
#5368=LINE('',#37035,#8237);
#5369=LINE('',#37037,#8238);
#5370=LINE('',#37039,#8239);
#5371=LINE('',#37041,#8240);
#5372=LINE('',#37043,#8241);
#5373=LINE('',#37045,#8242);
#5374=LINE('',#37047,#8243);
#5375=LINE('',#37049,#8244);
#5376=LINE('',#37051,#8245);
#5377=LINE('',#37053,#8246);
#5378=LINE('',#37055,#8247);
#5379=LINE('',#37057,#8248);
#5380=LINE('',#37058,#8249);
#5381=LINE('',#37060,#8250);
#5382=LINE('',#37062,#8251);
#5383=LINE('',#37064,#8252);
#5384=LINE('',#37066,#8253);
#5385=LINE('',#37068,#8254);
#5386=LINE('',#37070,#8255);
#5387=LINE('',#37072,#8256);
#5388=LINE('',#37074,#8257);
#5389=LINE('',#37076,#8258);
#5390=LINE('',#37078,#8259);
#5391=LINE('',#37080,#8260);
#5392=LINE('',#37082,#8261);
#5393=LINE('',#37084,#8262);
#5394=LINE('',#37086,#8263);
#5395=LINE('',#37088,#8264);
#5396=LINE('',#37090,#8265);
#5397=LINE('',#37092,#8266);
#5398=LINE('',#37094,#8267);
#5399=LINE('',#37095,#8268);
#5400=LINE('',#37097,#8269);
#5401=LINE('',#37099,#8270);
#5402=LINE('',#37101,#8271);
#5403=LINE('',#37103,#8272);
#5404=LINE('',#37105,#8273);
#5405=LINE('',#37107,#8274);
#5406=LINE('',#37109,#8275);
#5407=LINE('',#37111,#8276);
#5408=LINE('',#37113,#8277);
#5409=LINE('',#37115,#8278);
#5410=LINE('',#37117,#8279);
#5411=LINE('',#37119,#8280);
#5412=LINE('',#37121,#8281);
#5413=LINE('',#37123,#8282);
#5414=LINE('',#37125,#8283);
#5415=LINE('',#37127,#8284);
#5416=LINE('',#37129,#8285);
#5417=LINE('',#37131,#8286);
#5418=LINE('',#37132,#8287);
#5419=LINE('',#37134,#8288);
#5420=LINE('',#37136,#8289);
#5421=LINE('',#37138,#8290);
#5422=LINE('',#37140,#8291);
#5423=LINE('',#37142,#8292);
#5424=LINE('',#37144,#8293);
#5425=LINE('',#37146,#8294);
#5426=LINE('',#37148,#8295);
#5427=LINE('',#37150,#8296);
#5428=LINE('',#37152,#8297);
#5429=LINE('',#37154,#8298);
#5430=LINE('',#37156,#8299);
#5431=LINE('',#37158,#8300);
#5432=LINE('',#37160,#8301);
#5433=LINE('',#37162,#8302);
#5434=LINE('',#37164,#8303);
#5435=LINE('',#37166,#8304);
#5436=LINE('',#37168,#8305);
#5437=LINE('',#37169,#8306);
#5438=LINE('',#37171,#8307);
#5439=LINE('',#37173,#8308);
#5440=LINE('',#37175,#8309);
#5441=LINE('',#37177,#8310);
#5442=LINE('',#37179,#8311);
#5443=LINE('',#37181,#8312);
#5444=LINE('',#37183,#8313);
#5445=LINE('',#37185,#8314);
#5446=LINE('',#37187,#8315);
#5447=LINE('',#37189,#8316);
#5448=LINE('',#37191,#8317);
#5449=LINE('',#37193,#8318);
#5450=LINE('',#37195,#8319);
#5451=LINE('',#37197,#8320);
#5452=LINE('',#37199,#8321);
#5453=LINE('',#37201,#8322);
#5454=LINE('',#37203,#8323);
#5455=LINE('',#37205,#8324);
#5456=LINE('',#37206,#8325);
#5457=LINE('',#37208,#8326);
#5458=LINE('',#37210,#8327);
#5459=LINE('',#37212,#8328);
#5460=LINE('',#37214,#8329);
#5461=LINE('',#37216,#8330);
#5462=LINE('',#37218,#8331);
#5463=LINE('',#37220,#8332);
#5464=LINE('',#37222,#8333);
#5465=LINE('',#37224,#8334);
#5466=LINE('',#37226,#8335);
#5467=LINE('',#37228,#8336);
#5468=LINE('',#37230,#8337);
#5469=LINE('',#37232,#8338);
#5470=LINE('',#37234,#8339);
#5471=LINE('',#37236,#8340);
#5472=LINE('',#37238,#8341);
#5473=LINE('',#37240,#8342);
#5474=LINE('',#37242,#8343);
#5475=LINE('',#37243,#8344);
#5476=LINE('',#37245,#8345);
#5477=LINE('',#37247,#8346);
#5478=LINE('',#37249,#8347);
#5479=LINE('',#37251,#8348);
#5480=LINE('',#37253,#8349);
#5481=LINE('',#37255,#8350);
#5482=LINE('',#37257,#8351);
#5483=LINE('',#37259,#8352);
#5484=LINE('',#37261,#8353);
#5485=LINE('',#37263,#8354);
#5486=LINE('',#37265,#8355);
#5487=LINE('',#37267,#8356);
#5488=LINE('',#37269,#8357);
#5489=LINE('',#37271,#8358);
#5490=LINE('',#37273,#8359);
#5491=LINE('',#37275,#8360);
#5492=LINE('',#37277,#8361);
#5493=LINE('',#37279,#8362);
#5494=LINE('',#37280,#8363);
#5495=LINE('',#37282,#8364);
#5496=LINE('',#37284,#8365);
#5497=LINE('',#37286,#8366);
#5498=LINE('',#37288,#8367);
#5499=LINE('',#37290,#8368);
#5500=LINE('',#37292,#8369);
#5501=LINE('',#37294,#8370);
#5502=LINE('',#37296,#8371);
#5503=LINE('',#37298,#8372);
#5504=LINE('',#37300,#8373);
#5505=LINE('',#37302,#8374);
#5506=LINE('',#37304,#8375);
#5507=LINE('',#37306,#8376);
#5508=LINE('',#37308,#8377);
#5509=LINE('',#37310,#8378);
#5510=LINE('',#37312,#8379);
#5511=LINE('',#37314,#8380);
#5512=LINE('',#37316,#8381);
#5513=LINE('',#37317,#8382);
#5514=LINE('',#37319,#8383);
#5515=LINE('',#37321,#8384);
#5516=LINE('',#37323,#8385);
#5517=LINE('',#37325,#8386);
#5518=LINE('',#37327,#8387);
#5519=LINE('',#37329,#8388);
#5520=LINE('',#37331,#8389);
#5521=LINE('',#37333,#8390);
#5522=LINE('',#37335,#8391);
#5523=LINE('',#37337,#8392);
#5524=LINE('',#37339,#8393);
#5525=LINE('',#37341,#8394);
#5526=LINE('',#37343,#8395);
#5527=LINE('',#37345,#8396);
#5528=LINE('',#37347,#8397);
#5529=LINE('',#37349,#8398);
#5530=LINE('',#37351,#8399);
#5531=LINE('',#37353,#8400);
#5532=LINE('',#37354,#8401);
#5533=LINE('',#37356,#8402);
#5534=LINE('',#37358,#8403);
#5535=LINE('',#37360,#8404);
#5536=LINE('',#37362,#8405);
#5537=LINE('',#37364,#8406);
#5538=LINE('',#37366,#8407);
#5539=LINE('',#37368,#8408);
#5540=LINE('',#37370,#8409);
#5541=LINE('',#37372,#8410);
#5542=LINE('',#37374,#8411);
#5543=LINE('',#37376,#8412);
#5544=LINE('',#37378,#8413);
#5545=LINE('',#37380,#8414);
#5546=LINE('',#37382,#8415);
#5547=LINE('',#37384,#8416);
#5548=LINE('',#37386,#8417);
#5549=LINE('',#37388,#8418);
#5550=LINE('',#37390,#8419);
#5551=LINE('',#37391,#8420);
#5552=LINE('',#37393,#8421);
#5553=LINE('',#37395,#8422);
#5554=LINE('',#37397,#8423);
#5555=LINE('',#37399,#8424);
#5556=LINE('',#37401,#8425);
#5557=LINE('',#37403,#8426);
#5558=LINE('',#37405,#8427);
#5559=LINE('',#37407,#8428);
#5560=LINE('',#37409,#8429);
#5561=LINE('',#37411,#8430);
#5562=LINE('',#37413,#8431);
#5563=LINE('',#37415,#8432);
#5564=LINE('',#37417,#8433);
#5565=LINE('',#37419,#8434);
#5566=LINE('',#37421,#8435);
#5567=LINE('',#37423,#8436);
#5568=LINE('',#37425,#8437);
#5569=LINE('',#37427,#8438);
#5570=LINE('',#37428,#8439);
#5571=LINE('',#37430,#8440);
#5572=LINE('',#37432,#8441);
#5573=LINE('',#37434,#8442);
#5574=LINE('',#37436,#8443);
#5575=LINE('',#37438,#8444);
#5576=LINE('',#37440,#8445);
#5577=LINE('',#37442,#8446);
#5578=LINE('',#37444,#8447);
#5579=LINE('',#37446,#8448);
#5580=LINE('',#37448,#8449);
#5581=LINE('',#37450,#8450);
#5582=LINE('',#37452,#8451);
#5583=LINE('',#37454,#8452);
#5584=LINE('',#37456,#8453);
#5585=LINE('',#37458,#8454);
#5586=LINE('',#37460,#8455);
#5587=LINE('',#37462,#8456);
#5588=LINE('',#37464,#8457);
#5589=LINE('',#37465,#8458);
#5590=LINE('',#37470,#8459);
#5591=LINE('',#37471,#8460);
#5592=LINE('',#37472,#8461);
#5593=LINE('',#37475,#8462);
#5594=LINE('',#37477,#8463);
#5595=LINE('',#37478,#8464);
#5596=LINE('',#37481,#8465);
#5597=LINE('',#37482,#8466);
#5598=LINE('',#37483,#8467);
#5599=LINE('',#37486,#8468);
#5600=LINE('',#37488,#8469);
#5601=LINE('',#37489,#8470);
#5602=LINE('',#37492,#8471);
#5603=LINE('',#37493,#8472);
#5604=LINE('',#37494,#8473);
#5605=LINE('',#37497,#8474);
#5606=LINE('',#37499,#8475);
#5607=LINE('',#37500,#8476);
#5608=LINE('',#37503,#8477);
#5609=LINE('',#37504,#8478);
#5610=LINE('',#37505,#8479);
#5611=LINE('',#37508,#8480);
#5612=LINE('',#37510,#8481);
#5613=LINE('',#37511,#8482);
#5614=LINE('',#37514,#8483);
#5615=LINE('',#37515,#8484);
#5616=LINE('',#37516,#8485);
#5617=LINE('',#37519,#8486);
#5618=LINE('',#37521,#8487);
#5619=LINE('',#37522,#8488);
#5620=LINE('',#37525,#8489);
#5621=LINE('',#37526,#8490);
#5622=LINE('',#37527,#8491);
#5623=LINE('',#37530,#8492);
#5624=LINE('',#37532,#8493);
#5625=LINE('',#37533,#8494);
#5626=LINE('',#37536,#8495);
#5627=LINE('',#37537,#8496);
#5628=LINE('',#37538,#8497);
#5629=LINE('',#37541,#8498);
#5630=LINE('',#37543,#8499);
#5631=LINE('',#37544,#8500);
#5632=LINE('',#37547,#8501);
#5633=LINE('',#37548,#8502);
#5634=LINE('',#37549,#8503);
#5635=LINE('',#37552,#8504);
#5636=LINE('',#37554,#8505);
#5637=LINE('',#37555,#8506);
#5638=LINE('',#37558,#8507);
#5639=LINE('',#37559,#8508);
#5640=LINE('',#37560,#8509);
#5641=LINE('',#37563,#8510);
#5642=LINE('',#37565,#8511);
#5643=LINE('',#37566,#8512);
#5644=LINE('',#37569,#8513);
#5645=LINE('',#37570,#8514);
#5646=LINE('',#37571,#8515);
#5647=LINE('',#37574,#8516);
#5648=LINE('',#37576,#8517);
#5649=LINE('',#37577,#8518);
#5650=LINE('',#37580,#8519);
#5651=LINE('',#37581,#8520);
#5652=LINE('',#37582,#8521);
#5653=LINE('',#37585,#8522);
#5654=LINE('',#37587,#8523);
#5655=LINE('',#37588,#8524);
#5656=LINE('',#37591,#8525);
#5657=LINE('',#37592,#8526);
#5658=LINE('',#37593,#8527);
#5659=LINE('',#37599,#8528);
#5660=LINE('',#37601,#8529);
#5661=LINE('',#37602,#8530);
#5662=LINE('',#37605,#8531);
#5663=LINE('',#37607,#8532);
#5664=LINE('',#37608,#8533);
#5665=LINE('',#37611,#8534);
#5666=LINE('',#37613,#8535);
#5667=LINE('',#37614,#8536);
#5668=LINE('',#37617,#8537);
#5669=LINE('',#37620,#8538);
#5670=LINE('',#37621,#8539);
#5671=LINE('',#37623,#8540);
#5672=LINE('',#37626,#8541);
#5673=LINE('',#37628,#8542);
#5674=LINE('',#37630,#8543);
#5675=LINE('',#37632,#8544);
#5676=LINE('',#37634,#8545);
#5677=LINE('',#37636,#8546);
#5678=LINE('',#37638,#8547);
#5679=LINE('',#37640,#8548);
#5680=LINE('',#37642,#8549);
#5681=LINE('',#37644,#8550);
#5682=LINE('',#37646,#8551);
#5683=LINE('',#37648,#8552);
#5684=LINE('',#37650,#8553);
#5685=LINE('',#37652,#8554);
#5686=LINE('',#37654,#8555);
#5687=LINE('',#37657,#8556);
#5688=LINE('',#37659,#8557);
#5689=LINE('',#37661,#8558);
#5690=LINE('',#37664,#8559);
#5691=LINE('',#37666,#8560);
#5692=LINE('',#37668,#8561);
#5693=LINE('',#37670,#8562);
#5694=LINE('',#37672,#8563);
#5695=LINE('',#37674,#8564);
#5696=LINE('',#37676,#8565);
#5697=LINE('',#37678,#8566);
#5698=LINE('',#37680,#8567);
#5699=LINE('',#37682,#8568);
#5700=LINE('',#37684,#8569);
#5701=LINE('',#37686,#8570);
#5702=LINE('',#37688,#8571);
#5703=LINE('',#37690,#8572);
#5704=LINE('',#37692,#8573);
#5705=LINE('',#37695,#8574);
#5706=LINE('',#37697,#8575);
#5707=LINE('',#37699,#8576);
#5708=LINE('',#37702,#8577);
#5709=LINE('',#37704,#8578);
#5710=LINE('',#37706,#8579);
#5711=LINE('',#37708,#8580);
#5712=LINE('',#37710,#8581);
#5713=LINE('',#37712,#8582);
#5714=LINE('',#37714,#8583);
#5715=LINE('',#37716,#8584);
#5716=LINE('',#37718,#8585);
#5717=LINE('',#37720,#8586);
#5718=LINE('',#37722,#8587);
#5719=LINE('',#37724,#8588);
#5720=LINE('',#37726,#8589);
#5721=LINE('',#37728,#8590);
#5722=LINE('',#37730,#8591);
#5723=LINE('',#37733,#8592);
#5724=LINE('',#37735,#8593);
#5725=LINE('',#37737,#8594);
#5726=LINE('',#37740,#8595);
#5727=LINE('',#37742,#8596);
#5728=LINE('',#37744,#8597);
#5729=LINE('',#37746,#8598);
#5730=LINE('',#37748,#8599);
#5731=LINE('',#37750,#8600);
#5732=LINE('',#37752,#8601);
#5733=LINE('',#37754,#8602);
#5734=LINE('',#37756,#8603);
#5735=LINE('',#37758,#8604);
#5736=LINE('',#37760,#8605);
#5737=LINE('',#37762,#8606);
#5738=LINE('',#37764,#8607);
#5739=LINE('',#37766,#8608);
#5740=LINE('',#37768,#8609);
#5741=LINE('',#37771,#8610);
#5742=LINE('',#37773,#8611);
#5743=LINE('',#37775,#8612);
#5744=LINE('',#37778,#8613);
#5745=LINE('',#37780,#8614);
#5746=LINE('',#37782,#8615);
#5747=LINE('',#37784,#8616);
#5748=LINE('',#37786,#8617);
#5749=LINE('',#37788,#8618);
#5750=LINE('',#37790,#8619);
#5751=LINE('',#37792,#8620);
#5752=LINE('',#37794,#8621);
#5753=LINE('',#37796,#8622);
#5754=LINE('',#37798,#8623);
#5755=LINE('',#37800,#8624);
#5756=LINE('',#37802,#8625);
#5757=LINE('',#37804,#8626);
#5758=LINE('',#37806,#8627);
#5759=LINE('',#37809,#8628);
#5760=LINE('',#37811,#8629);
#5761=LINE('',#37813,#8630);
#5762=LINE('',#37816,#8631);
#5763=LINE('',#37818,#8632);
#5764=LINE('',#37820,#8633);
#5765=LINE('',#37822,#8634);
#5766=LINE('',#37824,#8635);
#5767=LINE('',#37826,#8636);
#5768=LINE('',#37828,#8637);
#5769=LINE('',#37830,#8638);
#5770=LINE('',#37832,#8639);
#5771=LINE('',#37834,#8640);
#5772=LINE('',#37836,#8641);
#5773=LINE('',#37838,#8642);
#5774=LINE('',#37840,#8643);
#5775=LINE('',#37842,#8644);
#5776=LINE('',#37844,#8645);
#5777=LINE('',#37847,#8646);
#5778=LINE('',#37849,#8647);
#5779=LINE('',#37851,#8648);
#5780=LINE('',#37854,#8649);
#5781=LINE('',#37856,#8650);
#5782=LINE('',#37858,#8651);
#5783=LINE('',#37860,#8652);
#5784=LINE('',#37862,#8653);
#5785=LINE('',#37864,#8654);
#5786=LINE('',#37866,#8655);
#5787=LINE('',#37868,#8656);
#5788=LINE('',#37870,#8657);
#5789=LINE('',#37872,#8658);
#5790=LINE('',#37874,#8659);
#5791=LINE('',#37876,#8660);
#5792=LINE('',#37878,#8661);
#5793=LINE('',#37880,#8662);
#5794=LINE('',#37882,#8663);
#5795=LINE('',#37885,#8664);
#5796=LINE('',#37887,#8665);
#5797=LINE('',#37889,#8666);
#5798=LINE('',#37892,#8667);
#5799=LINE('',#37894,#8668);
#5800=LINE('',#37896,#8669);
#5801=LINE('',#37898,#8670);
#5802=LINE('',#37900,#8671);
#5803=LINE('',#37902,#8672);
#5804=LINE('',#37904,#8673);
#5805=LINE('',#37906,#8674);
#5806=LINE('',#37908,#8675);
#5807=LINE('',#37910,#8676);
#5808=LINE('',#37912,#8677);
#5809=LINE('',#37914,#8678);
#5810=LINE('',#37916,#8679);
#5811=LINE('',#37918,#8680);
#5812=LINE('',#37920,#8681);
#5813=LINE('',#37923,#8682);
#5814=LINE('',#37925,#8683);
#5815=LINE('',#37927,#8684);
#5816=LINE('',#37930,#8685);
#5817=LINE('',#37932,#8686);
#5818=LINE('',#37934,#8687);
#5819=LINE('',#37936,#8688);
#5820=LINE('',#37938,#8689);
#5821=LINE('',#37940,#8690);
#5822=LINE('',#37942,#8691);
#5823=LINE('',#37944,#8692);
#5824=LINE('',#37946,#8693);
#5825=LINE('',#37948,#8694);
#5826=LINE('',#37950,#8695);
#5827=LINE('',#37952,#8696);
#5828=LINE('',#37954,#8697);
#5829=LINE('',#37956,#8698);
#5830=LINE('',#37958,#8699);
#5831=LINE('',#37961,#8700);
#5832=LINE('',#37963,#8701);
#5833=LINE('',#37965,#8702);
#5834=LINE('',#37968,#8703);
#5835=LINE('',#37970,#8704);
#5836=LINE('',#37972,#8705);
#5837=LINE('',#37974,#8706);
#5838=LINE('',#37976,#8707);
#5839=LINE('',#37978,#8708);
#5840=LINE('',#37980,#8709);
#5841=LINE('',#37982,#8710);
#5842=LINE('',#37984,#8711);
#5843=LINE('',#37986,#8712);
#5844=LINE('',#37988,#8713);
#5845=LINE('',#37990,#8714);
#5846=LINE('',#37992,#8715);
#5847=LINE('',#37994,#8716);
#5848=LINE('',#37996,#8717);
#5849=LINE('',#37999,#8718);
#5850=LINE('',#38001,#8719);
#5851=LINE('',#38003,#8720);
#5852=LINE('',#38006,#8721);
#5853=LINE('',#38008,#8722);
#5854=LINE('',#38010,#8723);
#5855=LINE('',#38012,#8724);
#5856=LINE('',#38014,#8725);
#5857=LINE('',#38016,#8726);
#5858=LINE('',#38018,#8727);
#5859=LINE('',#38020,#8728);
#5860=LINE('',#38022,#8729);
#5861=LINE('',#38024,#8730);
#5862=LINE('',#38026,#8731);
#5863=LINE('',#38028,#8732);
#5864=LINE('',#38030,#8733);
#5865=LINE('',#38032,#8734);
#5866=LINE('',#38034,#8735);
#5867=LINE('',#38037,#8736);
#5868=LINE('',#38039,#8737);
#5869=LINE('',#38041,#8738);
#5870=LINE('',#38044,#8739);
#5871=LINE('',#38046,#8740);
#5872=LINE('',#38048,#8741);
#5873=LINE('',#38050,#8742);
#5874=LINE('',#38052,#8743);
#5875=LINE('',#38054,#8744);
#5876=LINE('',#38056,#8745);
#5877=LINE('',#38058,#8746);
#5878=LINE('',#38060,#8747);
#5879=LINE('',#38062,#8748);
#5880=LINE('',#38064,#8749);
#5881=LINE('',#38066,#8750);
#5882=LINE('',#38068,#8751);
#5883=LINE('',#38070,#8752);
#5884=LINE('',#38072,#8753);
#5885=LINE('',#38077,#8754);
#5886=LINE('',#38085,#8755);
#5887=LINE('',#38089,#8756);
#5888=LINE('',#38094,#8757);
#5889=LINE('',#38100,#8758);
#5890=LINE('',#38102,#8759);
#5891=LINE('',#38104,#8760);
#5892=LINE('',#38106,#8761);
#5893=LINE('',#38108,#8762);
#5894=LINE('',#38109,#8763);
#5895=LINE('',#38112,#8764);
#5896=LINE('',#38114,#8765);
#5897=LINE('',#38116,#8766);
#5898=LINE('',#38118,#8767);
#5899=LINE('',#38120,#8768);
#5900=LINE('',#38122,#8769);
#5901=LINE('',#38124,#8770);
#5902=LINE('',#38126,#8771);
#5903=LINE('',#38128,#8772);
#5904=LINE('',#38130,#8773);
#5905=LINE('',#38132,#8774);
#5906=LINE('',#38134,#8775);
#5907=LINE('',#38136,#8776);
#5908=LINE('',#38138,#8777);
#5909=LINE('',#38140,#8778);
#5910=LINE('',#38142,#8779);
#5911=LINE('',#38144,#8780);
#5912=LINE('',#38146,#8781);
#5913=LINE('',#38148,#8782);
#5914=LINE('',#38150,#8783);
#5915=LINE('',#38152,#8784);
#5916=LINE('',#38154,#8785);
#5917=LINE('',#38156,#8786);
#5918=LINE('',#38158,#8787);
#5919=LINE('',#38160,#8788);
#5920=LINE('',#38162,#8789);
#5921=LINE('',#38164,#8790);
#5922=LINE('',#38166,#8791);
#5923=LINE('',#38168,#8792);
#5924=LINE('',#38170,#8793);
#5925=LINE('',#38172,#8794);
#5926=LINE('',#38174,#8795);
#5927=LINE('',#38176,#8796);
#5928=LINE('',#38178,#8797);
#5929=LINE('',#38180,#8798);
#5930=LINE('',#38182,#8799);
#5931=LINE('',#38184,#8800);
#5932=LINE('',#38186,#8801);
#5933=LINE('',#38188,#8802);
#5934=LINE('',#38190,#8803);
#5935=LINE('',#38192,#8804);
#5936=LINE('',#38194,#8805);
#5937=LINE('',#38196,#8806);
#5938=LINE('',#38198,#8807);
#5939=LINE('',#38200,#8808);
#5940=LINE('',#38202,#8809);
#5941=LINE('',#38204,#8810);
#5942=LINE('',#38206,#8811);
#5943=LINE('',#38208,#8812);
#5944=LINE('',#38210,#8813);
#5945=LINE('',#38212,#8814);
#5946=LINE('',#38214,#8815);
#5947=LINE('',#38216,#8816);
#5948=LINE('',#38218,#8817);
#5949=LINE('',#38220,#8818);
#5950=LINE('',#38222,#8819);
#5951=LINE('',#38224,#8820);
#5952=LINE('',#38226,#8821);
#5953=LINE('',#38228,#8822);
#5954=LINE('',#38230,#8823);
#5955=LINE('',#38232,#8824);
#5956=LINE('',#38234,#8825);
#5957=LINE('',#38236,#8826);
#5958=LINE('',#38238,#8827);
#5959=LINE('',#38240,#8828);
#5960=LINE('',#38242,#8829);
#5961=LINE('',#38244,#8830);
#5962=LINE('',#38246,#8831);
#5963=LINE('',#38248,#8832);
#5964=LINE('',#38250,#8833);
#5965=LINE('',#38252,#8834);
#5966=LINE('',#38254,#8835);
#5967=LINE('',#38256,#8836);
#5968=LINE('',#38258,#8837);
#5969=LINE('',#38260,#8838);
#5970=LINE('',#38262,#8839);
#5971=LINE('',#38264,#8840);
#5972=LINE('',#38266,#8841);
#5973=LINE('',#38268,#8842);
#5974=LINE('',#38270,#8843);
#5975=LINE('',#38272,#8844);
#5976=LINE('',#38274,#8845);
#5977=LINE('',#38276,#8846);
#5978=LINE('',#38278,#8847);
#5979=LINE('',#38280,#8848);
#5980=LINE('',#38282,#8849);
#5981=LINE('',#38284,#8850);
#5982=LINE('',#38286,#8851);
#5983=LINE('',#38288,#8852);
#5984=LINE('',#38290,#8853);
#5985=LINE('',#38292,#8854);
#5986=LINE('',#38294,#8855);
#5987=LINE('',#38296,#8856);
#5988=LINE('',#38298,#8857);
#5989=LINE('',#38300,#8858);
#5990=LINE('',#38302,#8859);
#5991=LINE('',#38304,#8860);
#5992=LINE('',#38306,#8861);
#5993=LINE('',#38308,#8862);
#5994=LINE('',#38310,#8863);
#5995=LINE('',#38312,#8864);
#5996=LINE('',#38314,#8865);
#5997=LINE('',#38316,#8866);
#5998=LINE('',#38318,#8867);
#5999=LINE('',#38320,#8868);
#6000=LINE('',#38322,#8869);
#6001=LINE('',#38324,#8870);
#6002=LINE('',#38326,#8871);
#6003=LINE('',#38328,#8872);
#6004=LINE('',#38330,#8873);
#6005=LINE('',#38332,#8874);
#6006=LINE('',#38334,#8875);
#6007=LINE('',#38336,#8876);
#6008=LINE('',#38338,#8877);
#6009=LINE('',#38340,#8878);
#6010=LINE('',#38342,#8879);
#6011=LINE('',#38344,#8880);
#6012=LINE('',#38346,#8881);
#6013=LINE('',#38348,#8882);
#6014=LINE('',#38350,#8883);
#6015=LINE('',#38352,#8884);
#6016=LINE('',#38354,#8885);
#6017=LINE('',#38356,#8886);
#6018=LINE('',#38358,#8887);
#6019=LINE('',#38360,#8888);
#6020=LINE('',#38362,#8889);
#6021=LINE('',#38364,#8890);
#6022=LINE('',#38366,#8891);
#6023=LINE('',#38368,#8892);
#6024=LINE('',#38370,#8893);
#6025=LINE('',#38372,#8894);
#6026=LINE('',#38374,#8895);
#6027=LINE('',#38376,#8896);
#6028=LINE('',#38378,#8897);
#6029=LINE('',#38380,#8898);
#6030=LINE('',#38382,#8899);
#6031=LINE('',#38384,#8900);
#6032=LINE('',#38386,#8901);
#6033=LINE('',#38388,#8902);
#6034=LINE('',#38390,#8903);
#6035=LINE('',#38392,#8904);
#6036=LINE('',#38394,#8905);
#6037=LINE('',#38396,#8906);
#6038=LINE('',#38398,#8907);
#6039=LINE('',#38400,#8908);
#6040=LINE('',#38402,#8909);
#6041=LINE('',#38404,#8910);
#6042=LINE('',#38406,#8911);
#6043=LINE('',#38408,#8912);
#6044=LINE('',#38410,#8913);
#6045=LINE('',#38412,#8914);
#6046=LINE('',#38414,#8915);
#6047=LINE('',#38416,#8916);
#6048=LINE('',#38418,#8917);
#6049=LINE('',#38420,#8918);
#6050=LINE('',#38422,#8919);
#6051=LINE('',#38424,#8920);
#6052=LINE('',#38426,#8921);
#6053=LINE('',#38428,#8922);
#6054=LINE('',#38430,#8923);
#6055=LINE('',#38432,#8924);
#6056=LINE('',#38434,#8925);
#6057=LINE('',#38436,#8926);
#6058=LINE('',#38438,#8927);
#6059=LINE('',#38440,#8928);
#6060=LINE('',#38442,#8929);
#6061=LINE('',#38444,#8930);
#6062=LINE('',#38446,#8931);
#6063=LINE('',#38448,#8932);
#6064=LINE('',#38450,#8933);
#6065=LINE('',#38452,#8934);
#6066=LINE('',#38454,#8935);
#6067=LINE('',#38456,#8936);
#6068=LINE('',#38458,#8937);
#6069=LINE('',#38460,#8938);
#6070=LINE('',#38462,#8939);
#6071=LINE('',#38464,#8940);
#6072=LINE('',#38466,#8941);
#6073=LINE('',#38468,#8942);
#6074=LINE('',#38470,#8943);
#6075=LINE('',#38472,#8944);
#6076=LINE('',#38474,#8945);
#6077=LINE('',#38476,#8946);
#6078=LINE('',#38478,#8947);
#6079=LINE('',#38480,#8948);
#6080=LINE('',#38482,#8949);
#6081=LINE('',#38484,#8950);
#6082=LINE('',#38486,#8951);
#6083=LINE('',#38488,#8952);
#6084=LINE('',#38490,#8953);
#6085=LINE('',#38492,#8954);
#6086=LINE('',#38494,#8955);
#6087=LINE('',#38496,#8956);
#6088=LINE('',#38498,#8957);
#6089=LINE('',#38500,#8958);
#6090=LINE('',#38502,#8959);
#6091=LINE('',#38504,#8960);
#6092=LINE('',#38506,#8961);
#6093=LINE('',#38508,#8962);
#6094=LINE('',#38510,#8963);
#6095=LINE('',#38512,#8964);
#6096=LINE('',#38514,#8965);
#6097=LINE('',#38516,#8966);
#6098=LINE('',#38518,#8967);
#6099=LINE('',#38520,#8968);
#6100=LINE('',#38522,#8969);
#6101=LINE('',#38524,#8970);
#6102=LINE('',#38526,#8971);
#6103=LINE('',#38528,#8972);
#6104=LINE('',#38530,#8973);
#6105=LINE('',#38532,#8974);
#6106=LINE('',#38534,#8975);
#6107=LINE('',#38536,#8976);
#6108=LINE('',#38538,#8977);
#6109=LINE('',#38540,#8978);
#6110=LINE('',#38542,#8979);
#6111=LINE('',#38544,#8980);
#6112=LINE('',#38546,#8981);
#6113=LINE('',#38548,#8982);
#6114=LINE('',#38550,#8983);
#6115=LINE('',#38552,#8984);
#6116=LINE('',#38554,#8985);
#6117=LINE('',#38556,#8986);
#6118=LINE('',#38558,#8987);
#6119=LINE('',#38560,#8988);
#6120=LINE('',#38562,#8989);
#6121=LINE('',#38564,#8990);
#6122=LINE('',#38566,#8991);
#6123=LINE('',#38568,#8992);
#6124=LINE('',#38570,#8993);
#6125=LINE('',#38572,#8994);
#6126=LINE('',#38574,#8995);
#6127=LINE('',#38576,#8996);
#6128=LINE('',#38578,#8997);
#6129=LINE('',#38580,#8998);
#6130=LINE('',#38582,#8999);
#6131=LINE('',#38584,#9000);
#6132=LINE('',#38586,#9001);
#6133=LINE('',#38587,#9002);
#6134=LINE('',#38592,#9003);
#6135=LINE('',#38594,#9004);
#6136=LINE('',#38596,#9005);
#6137=LINE('',#38597,#9006);
#6138=LINE('',#38600,#9007);
#6139=LINE('',#38601,#9008);
#6140=LINE('',#38604,#9009);
#6141=LINE('',#38606,#9010);
#6142=LINE('',#38608,#9011);
#6143=LINE('',#38610,#9012);
#6144=LINE('',#38611,#9013);
#6145=LINE('',#38614,#9014);
#6146=LINE('',#38616,#9015);
#6147=LINE('',#38618,#9016);
#6148=LINE('',#38619,#9017);
#6149=LINE('',#38622,#9018);
#6150=LINE('',#38623,#9019);
#6151=LINE('',#38626,#9020);
#6152=LINE('',#38628,#9021);
#6153=LINE('',#38630,#9022);
#6154=LINE('',#38632,#9023);
#6155=LINE('',#38633,#9024);
#6156=LINE('',#38636,#9025);
#6157=LINE('',#38638,#9026);
#6158=LINE('',#38640,#9027);
#6159=LINE('',#38641,#9028);
#6160=LINE('',#38644,#9029);
#6161=LINE('',#38645,#9030);
#6162=LINE('',#38648,#9031);
#6163=LINE('',#38650,#9032);
#6164=LINE('',#38652,#9033);
#6165=LINE('',#38654,#9034);
#6166=LINE('',#38655,#9035);
#6167=LINE('',#38658,#9036);
#6168=LINE('',#38660,#9037);
#6169=LINE('',#38662,#9038);
#6170=LINE('',#38663,#9039);
#6171=LINE('',#38666,#9040);
#6172=LINE('',#38667,#9041);
#6173=LINE('',#38670,#9042);
#6174=LINE('',#38672,#9043);
#6175=LINE('',#38674,#9044);
#6176=LINE('',#38676,#9045);
#6177=LINE('',#38677,#9046);
#6178=LINE('',#38680,#9047);
#6179=LINE('',#38682,#9048);
#6180=LINE('',#38684,#9049);
#6181=LINE('',#38685,#9050);
#6182=LINE('',#38688,#9051);
#6183=LINE('',#38689,#9052);
#6184=LINE('',#38692,#9053);
#6185=LINE('',#38694,#9054);
#6186=LINE('',#38696,#9055);
#6187=LINE('',#38698,#9056);
#6188=LINE('',#38699,#9057);
#6189=LINE('',#38702,#9058);
#6190=LINE('',#38704,#9059);
#6191=LINE('',#38706,#9060);
#6192=LINE('',#38707,#9061);
#6193=LINE('',#38710,#9062);
#6194=LINE('',#38711,#9063);
#6195=LINE('',#38714,#9064);
#6196=LINE('',#38716,#9065);
#6197=LINE('',#38718,#9066);
#6198=LINE('',#38720,#9067);
#6199=LINE('',#38721,#9068);
#6200=LINE('',#38724,#9069);
#6201=LINE('',#38726,#9070);
#6202=LINE('',#38728,#9071);
#6203=LINE('',#38729,#9072);
#6204=LINE('',#38732,#9073);
#6205=LINE('',#38733,#9074);
#6206=LINE('',#38736,#9075);
#6207=LINE('',#38738,#9076);
#6208=LINE('',#38740,#9077);
#6209=LINE('',#38742,#9078);
#6210=LINE('',#38743,#9079);
#6211=LINE('',#38746,#9080);
#6212=LINE('',#38748,#9081);
#6213=LINE('',#38750,#9082);
#6214=LINE('',#38751,#9083);
#6215=LINE('',#38754,#9084);
#6216=LINE('',#38755,#9085);
#6217=LINE('',#38758,#9086);
#6218=LINE('',#38760,#9087);
#6219=LINE('',#38762,#9088);
#6220=LINE('',#38764,#9089);
#6221=LINE('',#38765,#9090);
#6222=LINE('',#38768,#9091);
#6223=LINE('',#38770,#9092);
#6224=LINE('',#38772,#9093);
#6225=LINE('',#38773,#9094);
#6226=LINE('',#38776,#9095);
#6227=LINE('',#38777,#9096);
#6228=LINE('',#38780,#9097);
#6229=LINE('',#38782,#9098);
#6230=LINE('',#38784,#9099);
#6231=LINE('',#38786,#9100);
#6232=LINE('',#38787,#9101);
#6233=LINE('',#38790,#9102);
#6234=LINE('',#38792,#9103);
#6235=LINE('',#38794,#9104);
#6236=LINE('',#38795,#9105);
#6237=LINE('',#38798,#9106);
#6238=LINE('',#38799,#9107);
#6239=LINE('',#38802,#9108);
#6240=LINE('',#38804,#9109);
#6241=LINE('',#38806,#9110);
#6242=LINE('',#38808,#9111);
#6243=LINE('',#38809,#9112);
#6244=LINE('',#38812,#9113);
#6245=LINE('',#38814,#9114);
#6246=LINE('',#38816,#9115);
#6247=LINE('',#38817,#9116);
#6248=LINE('',#38820,#9117);
#6249=LINE('',#38821,#9118);
#6250=LINE('',#38824,#9119);
#6251=LINE('',#38826,#9120);
#6252=LINE('',#38828,#9121);
#6253=LINE('',#38830,#9122);
#6254=LINE('',#38831,#9123);
#6255=LINE('',#38834,#9124);
#6256=LINE('',#38836,#9125);
#6257=LINE('',#38838,#9126);
#6258=LINE('',#38839,#9127);
#6259=LINE('',#38842,#9128);
#6260=LINE('',#38843,#9129);
#6261=LINE('',#38847,#9130);
#6262=LINE('',#38849,#9131);
#6263=LINE('',#38850,#9132);
#6264=LINE('',#38852,#9133);
#6265=LINE('',#38853,#9134);
#6266=LINE('',#38856,#9135);
#6267=LINE('',#38858,#9136);
#6268=LINE('',#38859,#9137);
#6269=LINE('',#38862,#9138);
#6270=LINE('',#38863,#9139);
#6271=LINE('',#38867,#9140);
#6272=LINE('',#38869,#9141);
#6273=LINE('',#38870,#9142);
#6274=LINE('',#38872,#9143);
#6275=LINE('',#38873,#9144);
#6276=LINE('',#38876,#9145);
#6277=LINE('',#38878,#9146);
#6278=LINE('',#38879,#9147);
#6279=LINE('',#38882,#9148);
#6280=LINE('',#38883,#9149);
#6281=LINE('',#38887,#9150);
#6282=LINE('',#38889,#9151);
#6283=LINE('',#38890,#9152);
#6284=LINE('',#38892,#9153);
#6285=LINE('',#38893,#9154);
#6286=LINE('',#38896,#9155);
#6287=LINE('',#38898,#9156);
#6288=LINE('',#38899,#9157);
#6289=LINE('',#38902,#9158);
#6290=LINE('',#38903,#9159);
#6291=LINE('',#38907,#9160);
#6292=LINE('',#38909,#9161);
#6293=LINE('',#38910,#9162);
#6294=LINE('',#38912,#9163);
#6295=LINE('',#38913,#9164);
#6296=LINE('',#38916,#9165);
#6297=LINE('',#38918,#9166);
#6298=LINE('',#38919,#9167);
#6299=LINE('',#38922,#9168);
#6300=LINE('',#38923,#9169);
#6301=LINE('',#38927,#9170);
#6302=LINE('',#38929,#9171);
#6303=LINE('',#38930,#9172);
#6304=LINE('',#38932,#9173);
#6305=LINE('',#38933,#9174);
#6306=LINE('',#38936,#9175);
#6307=LINE('',#38938,#9176);
#6308=LINE('',#38939,#9177);
#6309=LINE('',#38942,#9178);
#6310=LINE('',#38943,#9179);
#6311=LINE('',#38947,#9180);
#6312=LINE('',#38949,#9181);
#6313=LINE('',#38950,#9182);
#6314=LINE('',#38952,#9183);
#6315=LINE('',#38953,#9184);
#6316=LINE('',#38956,#9185);
#6317=LINE('',#38958,#9186);
#6318=LINE('',#38959,#9187);
#6319=LINE('',#38962,#9188);
#6320=LINE('',#38963,#9189);
#6321=LINE('',#38967,#9190);
#6322=LINE('',#38969,#9191);
#6323=LINE('',#38970,#9192);
#6324=LINE('',#38972,#9193);
#6325=LINE('',#38973,#9194);
#6326=LINE('',#38976,#9195);
#6327=LINE('',#38978,#9196);
#6328=LINE('',#38979,#9197);
#6329=LINE('',#38982,#9198);
#6330=LINE('',#38983,#9199);
#6331=LINE('',#38987,#9200);
#6332=LINE('',#38989,#9201);
#6333=LINE('',#38990,#9202);
#6334=LINE('',#38992,#9203);
#6335=LINE('',#38993,#9204);
#6336=LINE('',#38996,#9205);
#6337=LINE('',#38998,#9206);
#6338=LINE('',#38999,#9207);
#6339=LINE('',#39002,#9208);
#6340=LINE('',#39003,#9209);
#6341=LINE('',#39007,#9210);
#6342=LINE('',#39009,#9211);
#6343=LINE('',#39010,#9212);
#6344=LINE('',#39012,#9213);
#6345=LINE('',#39013,#9214);
#6346=LINE('',#39016,#9215);
#6347=LINE('',#39018,#9216);
#6348=LINE('',#39019,#9217);
#6349=LINE('',#39022,#9218);
#6350=LINE('',#39023,#9219);
#6351=LINE('',#39027,#9220);
#6352=LINE('',#39029,#9221);
#6353=LINE('',#39030,#9222);
#6354=LINE('',#39032,#9223);
#6355=LINE('',#39033,#9224);
#6356=LINE('',#39036,#9225);
#6357=LINE('',#39038,#9226);
#6358=LINE('',#39039,#9227);
#6359=LINE('',#39042,#9228);
#6360=LINE('',#39043,#9229);
#6361=LINE('',#39047,#9230);
#6362=LINE('',#39049,#9231);
#6363=LINE('',#39050,#9232);
#6364=LINE('',#39052,#9233);
#6365=LINE('',#39053,#9234);
#6366=LINE('',#39056,#9235);
#6367=LINE('',#39058,#9236);
#6368=LINE('',#39059,#9237);
#6369=LINE('',#39062,#9238);
#6370=LINE('',#39063,#9239);
#6371=LINE('',#39067,#9240);
#6372=LINE('',#39069,#9241);
#6373=LINE('',#39070,#9242);
#6374=LINE('',#39072,#9243);
#6375=LINE('',#39073,#9244);
#6376=LINE('',#39076,#9245);
#6377=LINE('',#39078,#9246);
#6378=LINE('',#39079,#9247);
#6379=LINE('',#39082,#9248);
#6380=LINE('',#39083,#9249);
#6381=LINE('',#39086,#9250);
#6382=LINE('',#39088,#9251);
#6383=LINE('',#39090,#9252);
#6384=LINE('',#39091,#9253);
#6385=LINE('',#39094,#9254);
#6386=LINE('',#39096,#9255);
#6387=LINE('',#39098,#9256);
#6388=LINE('',#39100,#9257);
#6389=LINE('',#39102,#9258);
#6390=LINE('',#39104,#9259);
#6391=LINE('',#39106,#9260);
#6392=LINE('',#39108,#9261);
#6393=LINE('',#39110,#9262);
#6394=LINE('',#39112,#9263);
#6395=LINE('',#39114,#9264);
#6396=LINE('',#39116,#9265);
#6397=LINE('',#39118,#9266);
#6398=LINE('',#39120,#9267);
#6399=LINE('',#39122,#9268);
#6400=LINE('',#39124,#9269);
#6401=LINE('',#39126,#9270);
#6402=LINE('',#39127,#9271);
#6403=LINE('',#39129,#9272);
#6404=LINE('',#39131,#9273);
#6405=LINE('',#39133,#9274);
#6406=LINE('',#39135,#9275);
#6407=LINE('',#39137,#9276);
#6408=LINE('',#39139,#9277);
#6409=LINE('',#39141,#9278);
#6410=LINE('',#39143,#9279);
#6411=LINE('',#39145,#9280);
#6412=LINE('',#39147,#9281);
#6413=LINE('',#39149,#9282);
#6414=LINE('',#39151,#9283);
#6415=LINE('',#39153,#9284);
#6416=LINE('',#39155,#9285);
#6417=LINE('',#39157,#9286);
#6418=LINE('',#39159,#9287);
#6419=LINE('',#39161,#9288);
#6420=LINE('',#39163,#9289);
#6421=LINE('',#39164,#9290);
#6422=LINE('',#39166,#9291);
#6423=LINE('',#39168,#9292);
#6424=LINE('',#39170,#9293);
#6425=LINE('',#39172,#9294);
#6426=LINE('',#39174,#9295);
#6427=LINE('',#39176,#9296);
#6428=LINE('',#39178,#9297);
#6429=LINE('',#39180,#9298);
#6430=LINE('',#39182,#9299);
#6431=LINE('',#39184,#9300);
#6432=LINE('',#39186,#9301);
#6433=LINE('',#39188,#9302);
#6434=LINE('',#39190,#9303);
#6435=LINE('',#39192,#9304);
#6436=LINE('',#39194,#9305);
#6437=LINE('',#39196,#9306);
#6438=LINE('',#39198,#9307);
#6439=LINE('',#39200,#9308);
#6440=LINE('',#39201,#9309);
#6441=LINE('',#39203,#9310);
#6442=LINE('',#39205,#9311);
#6443=LINE('',#39207,#9312);
#6444=LINE('',#39209,#9313);
#6445=LINE('',#39211,#9314);
#6446=LINE('',#39213,#9315);
#6447=LINE('',#39215,#9316);
#6448=LINE('',#39217,#9317);
#6449=LINE('',#39219,#9318);
#6450=LINE('',#39221,#9319);
#6451=LINE('',#39223,#9320);
#6452=LINE('',#39225,#9321);
#6453=LINE('',#39227,#9322);
#6454=LINE('',#39229,#9323);
#6455=LINE('',#39231,#9324);
#6456=LINE('',#39233,#9325);
#6457=LINE('',#39235,#9326);
#6458=LINE('',#39237,#9327);
#6459=LINE('',#39238,#9328);
#6460=LINE('',#39240,#9329);
#6461=LINE('',#39242,#9330);
#6462=LINE('',#39244,#9331);
#6463=LINE('',#39246,#9332);
#6464=LINE('',#39248,#9333);
#6465=LINE('',#39250,#9334);
#6466=LINE('',#39252,#9335);
#6467=LINE('',#39254,#9336);
#6468=LINE('',#39256,#9337);
#6469=LINE('',#39258,#9338);
#6470=LINE('',#39260,#9339);
#6471=LINE('',#39262,#9340);
#6472=LINE('',#39264,#9341);
#6473=LINE('',#39266,#9342);
#6474=LINE('',#39268,#9343);
#6475=LINE('',#39270,#9344);
#6476=LINE('',#39272,#9345);
#6477=LINE('',#39274,#9346);
#6478=LINE('',#39275,#9347);
#6479=LINE('',#39277,#9348);
#6480=LINE('',#39279,#9349);
#6481=LINE('',#39281,#9350);
#6482=LINE('',#39283,#9351);
#6483=LINE('',#39285,#9352);
#6484=LINE('',#39287,#9353);
#6485=LINE('',#39289,#9354);
#6486=LINE('',#39291,#9355);
#6487=LINE('',#39293,#9356);
#6488=LINE('',#39295,#9357);
#6489=LINE('',#39297,#9358);
#6490=LINE('',#39299,#9359);
#6491=LINE('',#39301,#9360);
#6492=LINE('',#39303,#9361);
#6493=LINE('',#39305,#9362);
#6494=LINE('',#39307,#9363);
#6495=LINE('',#39309,#9364);
#6496=LINE('',#39311,#9365);
#6497=LINE('',#39312,#9366);
#6498=LINE('',#39314,#9367);
#6499=LINE('',#39316,#9368);
#6500=LINE('',#39318,#9369);
#6501=LINE('',#39320,#9370);
#6502=LINE('',#39322,#9371);
#6503=LINE('',#39324,#9372);
#6504=LINE('',#39326,#9373);
#6505=LINE('',#39328,#9374);
#6506=LINE('',#39330,#9375);
#6507=LINE('',#39332,#9376);
#6508=LINE('',#39334,#9377);
#6509=LINE('',#39336,#9378);
#6510=LINE('',#39338,#9379);
#6511=LINE('',#39340,#9380);
#6512=LINE('',#39342,#9381);
#6513=LINE('',#39344,#9382);
#6514=LINE('',#39346,#9383);
#6515=LINE('',#39348,#9384);
#6516=LINE('',#39349,#9385);
#6517=LINE('',#39351,#9386);
#6518=LINE('',#39353,#9387);
#6519=LINE('',#39355,#9388);
#6520=LINE('',#39357,#9389);
#6521=LINE('',#39359,#9390);
#6522=LINE('',#39361,#9391);
#6523=LINE('',#39363,#9392);
#6524=LINE('',#39365,#9393);
#6525=LINE('',#39367,#9394);
#6526=LINE('',#39369,#9395);
#6527=LINE('',#39371,#9396);
#6528=LINE('',#39373,#9397);
#6529=LINE('',#39375,#9398);
#6530=LINE('',#39377,#9399);
#6531=LINE('',#39379,#9400);
#6532=LINE('',#39381,#9401);
#6533=LINE('',#39383,#9402);
#6534=LINE('',#39385,#9403);
#6535=LINE('',#39386,#9404);
#6536=LINE('',#39388,#9405);
#6537=LINE('',#39390,#9406);
#6538=LINE('',#39392,#9407);
#6539=LINE('',#39394,#9408);
#6540=LINE('',#39396,#9409);
#6541=LINE('',#39398,#9410);
#6542=LINE('',#39400,#9411);
#6543=LINE('',#39402,#9412);
#6544=LINE('',#39404,#9413);
#6545=LINE('',#39406,#9414);
#6546=LINE('',#39408,#9415);
#6547=LINE('',#39410,#9416);
#6548=LINE('',#39412,#9417);
#6549=LINE('',#39414,#9418);
#6550=LINE('',#39416,#9419);
#6551=LINE('',#39418,#9420);
#6552=LINE('',#39420,#9421);
#6553=LINE('',#39422,#9422);
#6554=LINE('',#39423,#9423);
#6555=LINE('',#39425,#9424);
#6556=LINE('',#39427,#9425);
#6557=LINE('',#39429,#9426);
#6558=LINE('',#39431,#9427);
#6559=LINE('',#39433,#9428);
#6560=LINE('',#39435,#9429);
#6561=LINE('',#39437,#9430);
#6562=LINE('',#39439,#9431);
#6563=LINE('',#39441,#9432);
#6564=LINE('',#39443,#9433);
#6565=LINE('',#39445,#9434);
#6566=LINE('',#39447,#9435);
#6567=LINE('',#39449,#9436);
#6568=LINE('',#39451,#9437);
#6569=LINE('',#39453,#9438);
#6570=LINE('',#39455,#9439);
#6571=LINE('',#39457,#9440);
#6572=LINE('',#39459,#9441);
#6573=LINE('',#39460,#9442);
#6574=LINE('',#39462,#9443);
#6575=LINE('',#39464,#9444);
#6576=LINE('',#39466,#9445);
#6577=LINE('',#39468,#9446);
#6578=LINE('',#39470,#9447);
#6579=LINE('',#39472,#9448);
#6580=LINE('',#39474,#9449);
#6581=LINE('',#39476,#9450);
#6582=LINE('',#39478,#9451);
#6583=LINE('',#39480,#9452);
#6584=LINE('',#39482,#9453);
#6585=LINE('',#39484,#9454);
#6586=LINE('',#39486,#9455);
#6587=LINE('',#39488,#9456);
#6588=LINE('',#39490,#9457);
#6589=LINE('',#39492,#9458);
#6590=LINE('',#39494,#9459);
#6591=LINE('',#39496,#9460);
#6592=LINE('',#39497,#9461);
#6593=LINE('',#39499,#9462);
#6594=LINE('',#39501,#9463);
#6595=LINE('',#39503,#9464);
#6596=LINE('',#39505,#9465);
#6597=LINE('',#39507,#9466);
#6598=LINE('',#39509,#9467);
#6599=LINE('',#39511,#9468);
#6600=LINE('',#39513,#9469);
#6601=LINE('',#39515,#9470);
#6602=LINE('',#39517,#9471);
#6603=LINE('',#39519,#9472);
#6604=LINE('',#39521,#9473);
#6605=LINE('',#39523,#9474);
#6606=LINE('',#39525,#9475);
#6607=LINE('',#39527,#9476);
#6608=LINE('',#39529,#9477);
#6609=LINE('',#39531,#9478);
#6610=LINE('',#39533,#9479);
#6611=LINE('',#39534,#9480);
#6612=LINE('',#39539,#9481);
#6613=LINE('',#39540,#9482);
#6614=LINE('',#39541,#9483);
#6615=LINE('',#39544,#9484);
#6616=LINE('',#39546,#9485);
#6617=LINE('',#39547,#9486);
#6618=LINE('',#39550,#9487);
#6619=LINE('',#39551,#9488);
#6620=LINE('',#39552,#9489);
#6621=LINE('',#39555,#9490);
#6622=LINE('',#39557,#9491);
#6623=LINE('',#39558,#9492);
#6624=LINE('',#39561,#9493);
#6625=LINE('',#39562,#9494);
#6626=LINE('',#39563,#9495);
#6627=LINE('',#39566,#9496);
#6628=LINE('',#39568,#9497);
#6629=LINE('',#39569,#9498);
#6630=LINE('',#39572,#9499);
#6631=LINE('',#39573,#9500);
#6632=LINE('',#39574,#9501);
#6633=LINE('',#39577,#9502);
#6634=LINE('',#39579,#9503);
#6635=LINE('',#39580,#9504);
#6636=LINE('',#39583,#9505);
#6637=LINE('',#39584,#9506);
#6638=LINE('',#39585,#9507);
#6639=LINE('',#39588,#9508);
#6640=LINE('',#39590,#9509);
#6641=LINE('',#39591,#9510);
#6642=LINE('',#39594,#9511);
#6643=LINE('',#39595,#9512);
#6644=LINE('',#39596,#9513);
#6645=LINE('',#39599,#9514);
#6646=LINE('',#39601,#9515);
#6647=LINE('',#39602,#9516);
#6648=LINE('',#39605,#9517);
#6649=LINE('',#39606,#9518);
#6650=LINE('',#39607,#9519);
#6651=LINE('',#39610,#9520);
#6652=LINE('',#39612,#9521);
#6653=LINE('',#39613,#9522);
#6654=LINE('',#39616,#9523);
#6655=LINE('',#39617,#9524);
#6656=LINE('',#39618,#9525);
#6657=LINE('',#39621,#9526);
#6658=LINE('',#39623,#9527);
#6659=LINE('',#39624,#9528);
#6660=LINE('',#39627,#9529);
#6661=LINE('',#39628,#9530);
#6662=LINE('',#39629,#9531);
#6663=LINE('',#39632,#9532);
#6664=LINE('',#39634,#9533);
#6665=LINE('',#39635,#9534);
#6666=LINE('',#39638,#9535);
#6667=LINE('',#39639,#9536);
#6668=LINE('',#39640,#9537);
#6669=LINE('',#39643,#9538);
#6670=LINE('',#39645,#9539);
#6671=LINE('',#39646,#9540);
#6672=LINE('',#39649,#9541);
#6673=LINE('',#39650,#9542);
#6674=LINE('',#39651,#9543);
#6675=LINE('',#39654,#9544);
#6676=LINE('',#39656,#9545);
#6677=LINE('',#39657,#9546);
#6678=LINE('',#39660,#9547);
#6679=LINE('',#39661,#9548);
#6680=LINE('',#39662,#9549);
#6681=LINE('',#39664,#9550);
#6682=LINE('',#39665,#9551);
#6683=LINE('',#39667,#9552);
#6684=LINE('',#39670,#9553);
#6685=LINE('',#39672,#9554);
#6686=LINE('',#39674,#9555);
#6687=LINE('',#39676,#9556);
#6688=LINE('',#39678,#9557);
#6689=LINE('',#39680,#9558);
#6690=LINE('',#39682,#9559);
#6691=LINE('',#39684,#9560);
#6692=LINE('',#39686,#9561);
#6693=LINE('',#39688,#9562);
#6694=LINE('',#39690,#9563);
#6695=LINE('',#39692,#9564);
#6696=LINE('',#39694,#9565);
#6697=LINE('',#39696,#9566);
#6698=LINE('',#39698,#9567);
#6699=LINE('',#39701,#9568);
#6700=LINE('',#39703,#9569);
#6701=LINE('',#39705,#9570);
#6702=LINE('',#39708,#9571);
#6703=LINE('',#39710,#9572);
#6704=LINE('',#39712,#9573);
#6705=LINE('',#39714,#9574);
#6706=LINE('',#39716,#9575);
#6707=LINE('',#39718,#9576);
#6708=LINE('',#39720,#9577);
#6709=LINE('',#39722,#9578);
#6710=LINE('',#39724,#9579);
#6711=LINE('',#39726,#9580);
#6712=LINE('',#39728,#9581);
#6713=LINE('',#39730,#9582);
#6714=LINE('',#39732,#9583);
#6715=LINE('',#39734,#9584);
#6716=LINE('',#39736,#9585);
#6717=LINE('',#39739,#9586);
#6718=LINE('',#39741,#9587);
#6719=LINE('',#39743,#9588);
#6720=LINE('',#39746,#9589);
#6721=LINE('',#39748,#9590);
#6722=LINE('',#39750,#9591);
#6723=LINE('',#39752,#9592);
#6724=LINE('',#39754,#9593);
#6725=LINE('',#39756,#9594);
#6726=LINE('',#39758,#9595);
#6727=LINE('',#39760,#9596);
#6728=LINE('',#39762,#9597);
#6729=LINE('',#39764,#9598);
#6730=LINE('',#39766,#9599);
#6731=LINE('',#39768,#9600);
#6732=LINE('',#39770,#9601);
#6733=LINE('',#39772,#9602);
#6734=LINE('',#39774,#9603);
#6735=LINE('',#39777,#9604);
#6736=LINE('',#39779,#9605);
#6737=LINE('',#39781,#9606);
#6738=LINE('',#39784,#9607);
#6739=LINE('',#39786,#9608);
#6740=LINE('',#39788,#9609);
#6741=LINE('',#39790,#9610);
#6742=LINE('',#39792,#9611);
#6743=LINE('',#39794,#9612);
#6744=LINE('',#39796,#9613);
#6745=LINE('',#39798,#9614);
#6746=LINE('',#39800,#9615);
#6747=LINE('',#39802,#9616);
#6748=LINE('',#39804,#9617);
#6749=LINE('',#39806,#9618);
#6750=LINE('',#39808,#9619);
#6751=LINE('',#39810,#9620);
#6752=LINE('',#39812,#9621);
#6753=LINE('',#39815,#9622);
#6754=LINE('',#39817,#9623);
#6755=LINE('',#39819,#9624);
#6756=LINE('',#39822,#9625);
#6757=LINE('',#39824,#9626);
#6758=LINE('',#39826,#9627);
#6759=LINE('',#39828,#9628);
#6760=LINE('',#39830,#9629);
#6761=LINE('',#39832,#9630);
#6762=LINE('',#39834,#9631);
#6763=LINE('',#39836,#9632);
#6764=LINE('',#39838,#9633);
#6765=LINE('',#39840,#9634);
#6766=LINE('',#39842,#9635);
#6767=LINE('',#39844,#9636);
#6768=LINE('',#39846,#9637);
#6769=LINE('',#39848,#9638);
#6770=LINE('',#39850,#9639);
#6771=LINE('',#39853,#9640);
#6772=LINE('',#39855,#9641);
#6773=LINE('',#39857,#9642);
#6774=LINE('',#39860,#9643);
#6775=LINE('',#39862,#9644);
#6776=LINE('',#39864,#9645);
#6777=LINE('',#39866,#9646);
#6778=LINE('',#39868,#9647);
#6779=LINE('',#39870,#9648);
#6780=LINE('',#39872,#9649);
#6781=LINE('',#39874,#9650);
#6782=LINE('',#39876,#9651);
#6783=LINE('',#39878,#9652);
#6784=LINE('',#39880,#9653);
#6785=LINE('',#39882,#9654);
#6786=LINE('',#39884,#9655);
#6787=LINE('',#39886,#9656);
#6788=LINE('',#39888,#9657);
#6789=LINE('',#39891,#9658);
#6790=LINE('',#39893,#9659);
#6791=LINE('',#39895,#9660);
#6792=LINE('',#39898,#9661);
#6793=LINE('',#39900,#9662);
#6794=LINE('',#39902,#9663);
#6795=LINE('',#39904,#9664);
#6796=LINE('',#39906,#9665);
#6797=LINE('',#39908,#9666);
#6798=LINE('',#39910,#9667);
#6799=LINE('',#39912,#9668);
#6800=LINE('',#39914,#9669);
#6801=LINE('',#39916,#9670);
#6802=LINE('',#39918,#9671);
#6803=LINE('',#39920,#9672);
#6804=LINE('',#39922,#9673);
#6805=LINE('',#39924,#9674);
#6806=LINE('',#39926,#9675);
#6807=LINE('',#39929,#9676);
#6808=LINE('',#39931,#9677);
#6809=LINE('',#39933,#9678);
#6810=LINE('',#39936,#9679);
#6811=LINE('',#39938,#9680);
#6812=LINE('',#39940,#9681);
#6813=LINE('',#39942,#9682);
#6814=LINE('',#39944,#9683);
#6815=LINE('',#39946,#9684);
#6816=LINE('',#39948,#9685);
#6817=LINE('',#39950,#9686);
#6818=LINE('',#39952,#9687);
#6819=LINE('',#39954,#9688);
#6820=LINE('',#39956,#9689);
#6821=LINE('',#39958,#9690);
#6822=LINE('',#39960,#9691);
#6823=LINE('',#39962,#9692);
#6824=LINE('',#39964,#9693);
#6825=LINE('',#39967,#9694);
#6826=LINE('',#39969,#9695);
#6827=LINE('',#39971,#9696);
#6828=LINE('',#39974,#9697);
#6829=LINE('',#39976,#9698);
#6830=LINE('',#39978,#9699);
#6831=LINE('',#39980,#9700);
#6832=LINE('',#39982,#9701);
#6833=LINE('',#39984,#9702);
#6834=LINE('',#39986,#9703);
#6835=LINE('',#39988,#9704);
#6836=LINE('',#39990,#9705);
#6837=LINE('',#39992,#9706);
#6838=LINE('',#39994,#9707);
#6839=LINE('',#39996,#9708);
#6840=LINE('',#39998,#9709);
#6841=LINE('',#40000,#9710);
#6842=LINE('',#40002,#9711);
#6843=LINE('',#40005,#9712);
#6844=LINE('',#40007,#9713);
#6845=LINE('',#40009,#9714);
#6846=LINE('',#40012,#9715);
#6847=LINE('',#40014,#9716);
#6848=LINE('',#40016,#9717);
#6849=LINE('',#40018,#9718);
#6850=LINE('',#40020,#9719);
#6851=LINE('',#40022,#9720);
#6852=LINE('',#40024,#9721);
#6853=LINE('',#40026,#9722);
#6854=LINE('',#40028,#9723);
#6855=LINE('',#40030,#9724);
#6856=LINE('',#40032,#9725);
#6857=LINE('',#40034,#9726);
#6858=LINE('',#40036,#9727);
#6859=LINE('',#40038,#9728);
#6860=LINE('',#40040,#9729);
#6861=LINE('',#40043,#9730);
#6862=LINE('',#40045,#9731);
#6863=LINE('',#40047,#9732);
#6864=LINE('',#40050,#9733);
#6865=LINE('',#40052,#9734);
#6866=LINE('',#40054,#9735);
#6867=LINE('',#40056,#9736);
#6868=LINE('',#40058,#9737);
#6869=LINE('',#40060,#9738);
#6870=LINE('',#40062,#9739);
#6871=LINE('',#40064,#9740);
#6872=LINE('',#40066,#9741);
#6873=LINE('',#40068,#9742);
#6874=LINE('',#40070,#9743);
#6875=LINE('',#40072,#9744);
#6876=LINE('',#40074,#9745);
#6877=LINE('',#40076,#9746);
#6878=LINE('',#40078,#9747);
#6879=LINE('',#40081,#9748);
#6880=LINE('',#40083,#9749);
#6881=LINE('',#40085,#9750);
#6882=LINE('',#40088,#9751);
#6883=LINE('',#40090,#9752);
#6884=LINE('',#40092,#9753);
#6885=LINE('',#40094,#9754);
#6886=LINE('',#40096,#9755);
#6887=LINE('',#40098,#9756);
#6888=LINE('',#40100,#9757);
#6889=LINE('',#40102,#9758);
#6890=LINE('',#40104,#9759);
#6891=LINE('',#40106,#9760);
#6892=LINE('',#40108,#9761);
#6893=LINE('',#40110,#9762);
#6894=LINE('',#40112,#9763);
#6895=LINE('',#40114,#9764);
#6896=LINE('',#40116,#9765);
#6897=LINE('',#40121,#9766);
#6898=LINE('',#40127,#9767);
#6899=LINE('',#40133,#9768);
#6900=LINE('',#40135,#9769);
#6901=LINE('',#40137,#9770);
#6902=LINE('',#40138,#9771);
#6903=LINE('',#40141,#9772);
#6904=LINE('',#40143,#9773);
#6905=LINE('',#40144,#9774);
#6906=LINE('',#40147,#9775);
#6907=LINE('',#40149,#9776);
#6908=LINE('',#40150,#9777);
#6909=LINE('',#40152,#9778);
#6910=LINE('',#40153,#9779);
#6911=LINE('',#40158,#9780);
#6912=LINE('',#40160,#9781);
#6913=LINE('',#40162,#9782);
#6914=LINE('',#40163,#9783);
#6915=LINE('',#40166,#9784);
#6916=LINE('',#40168,#9785);
#6917=LINE('',#40169,#9786);
#6918=LINE('',#40172,#9787);
#6919=LINE('',#40174,#9788);
#6920=LINE('',#40175,#9789);
#6921=LINE('',#40177,#9790);
#6922=LINE('',#40178,#9791);
#6923=LINE('',#40184,#9792);
#6924=LINE('',#40190,#9793);
#6925=LINE('',#40197,#9794);
#6926=LINE('',#40200,#9795);
#6927=LINE('',#40213,#9796);
#6928=LINE('',#40221,#9797);
#6929=LINE('',#40225,#9798);
#6930=LINE('',#40232,#9799);
#6931=LINE('',#40238,#9800);
#6932=LINE('',#40244,#9801);
#6933=LINE('',#40249,#9802);
#6934=LINE('',#40253,#9803);
#6935=LINE('',#40269,#9804);
#6936=LINE('',#40272,#9805);
#6937=LINE('',#40275,#9806);
#6938=LINE('',#40277,#9807);
#6939=LINE('',#40278,#9808);
#6940=LINE('',#40281,#9809);
#6941=LINE('',#40285,#9810);
#6942=LINE('',#40286,#9811);
#6943=LINE('',#40291,#9812);
#6944=LINE('',#40305,#9813);
#6945=LINE('',#40317,#9814);
#6946=LINE('',#40321,#9815);
#6947=LINE('',#40326,#9816);
#6948=LINE('',#40332,#9817);
#6949=LINE('',#40336,#9818);
#6950=LINE('',#40339,#9819);
#6951=LINE('',#40344,#9820);
#6952=LINE('',#40346,#9821);
#6953=LINE('',#40348,#9822);
#6954=LINE('',#40350,#9823);
#6955=LINE('',#40352,#9824);
#6956=LINE('',#40353,#9825);
#6957=LINE('',#40356,#9826);
#6958=LINE('',#40358,#9827);
#6959=LINE('',#40359,#9828);
#6960=LINE('',#40362,#9829);
#6961=LINE('',#40364,#9830);
#6962=LINE('',#40366,#9831);
#6963=LINE('',#40367,#9832);
#6964=LINE('',#40370,#9833);
#6965=LINE('',#40372,#9834);
#6966=LINE('',#40374,#9835);
#6967=LINE('',#40375,#9836);
#6968=LINE('',#40378,#9837);
#6969=LINE('',#40380,#9838);
#6970=LINE('',#40382,#9839);
#6971=LINE('',#40384,#9840);
#6972=LINE('',#40385,#9841);
#6973=LINE('',#40388,#9842);
#6974=LINE('',#40390,#9843);
#6975=LINE('',#40391,#9844);
#6976=LINE('',#40394,#9845);
#6977=LINE('',#40396,#9846);
#6978=LINE('',#40398,#9847);
#6979=LINE('',#40399,#9848);
#6980=LINE('',#40402,#9849);
#6981=LINE('',#40403,#9850);
#6982=LINE('',#40404,#9851);
#6983=LINE('',#40407,#9852);
#6984=LINE('',#40408,#9853);
#6985=LINE('',#40411,#9854);
#6986=LINE('',#40413,#9855);
#6987=LINE('',#40415,#9856);
#6988=LINE('',#40416,#9857);
#6989=LINE('',#40419,#9858);
#6990=LINE('',#40420,#9859);
#6991=LINE('',#40421,#9860);
#6992=LINE('',#40424,#9861);
#6993=LINE('',#40425,#9862);
#6994=LINE('',#40428,#9863);
#6995=LINE('',#40430,#9864);
#6996=LINE('',#40431,#9865);
#6997=LINE('',#40433,#9866);
#6998=LINE('',#40435,#9867);
#6999=LINE('',#40452,#9868);
#7000=LINE('',#40463,#9869);
#7001=LINE('',#40468,#9870);
#7002=LINE('',#40470,#9871);
#7003=LINE('',#40471,#9872);
#7004=LINE('',#40475,#9873);
#7005=LINE('',#40477,#9874);
#7006=LINE('',#40478,#9875);
#7007=LINE('',#40482,#9876);
#7008=LINE('',#40484,#9877);
#7009=LINE('',#40485,#9878);
#7010=LINE('',#40489,#9879);
#7011=LINE('',#40491,#9880);
#7012=LINE('',#40492,#9881);
#7013=LINE('',#40494,#9882);
#7014=LINE('',#40495,#9883);
#7015=LINE('',#40499,#9884);
#7016=LINE('',#40501,#9885);
#7017=LINE('',#40502,#9886);
#7018=LINE('',#40506,#9887);
#7019=LINE('',#40508,#9888);
#7020=LINE('',#40509,#9889);
#7021=LINE('',#40511,#9890);
#7022=LINE('',#40512,#9891);
#7023=LINE('',#40514,#9892);
#7024=LINE('',#40515,#9893);
#7025=LINE('',#40522,#9894);
#7026=LINE('',#40523,#9895);
#7027=LINE('',#40525,#9896);
#7028=LINE('',#40526,#9897);
#7029=LINE('',#40533,#9898);
#7030=LINE('',#40534,#9899);
#7031=LINE('',#40541,#9900);
#7032=LINE('',#40542,#9901);
#7033=LINE('',#40544,#9902);
#7034=LINE('',#40545,#9903);
#7035=LINE('',#40552,#9904);
#7036=LINE('',#40553,#9905);
#7037=LINE('',#40560,#9906);
#7038=LINE('',#40561,#9907);
#7039=LINE('',#40563,#9908);
#7040=LINE('',#40564,#9909);
#7041=LINE('',#40571,#9910);
#7042=LINE('',#40572,#9911);
#7043=LINE('',#40595,#9912);
#7044=LINE('',#40597,#9913);
#7045=LINE('',#40599,#9914);
#7046=LINE('',#40600,#9915);
#7047=LINE('',#40603,#9916);
#7048=LINE('',#40605,#9917);
#7049=LINE('',#40606,#9918);
#7050=LINE('',#40610,#9919);
#7051=LINE('',#40612,#9920);
#7052=LINE('',#40614,#9921);
#7053=LINE('',#40615,#9922);
#7054=LINE('',#40618,#9923);
#7055=LINE('',#40620,#9924);
#7056=LINE('',#40621,#9925);
#7057=LINE('',#40623,#9926);
#7058=LINE('',#40624,#9927);
#7059=LINE('',#40626,#9928);
#7060=LINE('',#40627,#9929);
#7061=LINE('',#40630,#9930);
#7062=LINE('',#40632,#9931);
#7063=LINE('',#40633,#9932);
#7064=LINE('',#40636,#9933);
#7065=LINE('',#40637,#9934);
#7066=LINE('',#40640,#9935);
#7067=LINE('',#40641,#9936);
#7068=LINE('',#40647,#9937);
#7069=LINE('',#40648,#9938);
#7070=LINE('',#40651,#9939);
#7071=LINE('',#40652,#9940);
#7072=LINE('',#40654,#9941);
#7073=LINE('',#40657,#9942);
#7074=LINE('',#40676,#9943);
#7075=LINE('',#40680,#9944);
#7076=LINE('',#40685,#9945);
#7077=LINE('',#40691,#9946);
#7078=LINE('',#40702,#9947);
#7079=LINE('',#40707,#9948);
#7080=LINE('',#40715,#9949);
#7081=LINE('',#40721,#9950);
#7082=LINE('',#40726,#9951);
#7083=LINE('',#40733,#9952);
#7084=LINE('',#40766,#9953);
#7085=LINE('',#40850,#9954);
#7086=LINE('',#40940,#9955);
#7087=LINE('',#41030,#9956);
#7088=LINE('',#41114,#9957);
#7089=LINE('',#41204,#9958);
#7090=LINE('',#41294,#9959);
#7091=LINE('',#41378,#9960);
#7092=LINE('',#41468,#9961);
#7093=LINE('',#41546,#9962);
#7094=LINE('',#41594,#9963);
#7095=LINE('',#41648,#9964);
#7096=LINE('',#41732,#9965);
#7097=LINE('',#41816,#9966);
#7098=LINE('',#41906,#9967);
#7099=LINE('',#41996,#9968);
#7100=LINE('',#42080,#9969);
#7101=LINE('',#42170,#9970);
#7102=LINE('',#42260,#9971);
#7103=LINE('',#42344,#9972);
#7104=LINE('',#42430,#9973);
#7105=LINE('',#42456,#9974);
#7106=LINE('',#42493,#9975);
#7107=LINE('',#42530,#9976);
#7108=LINE('',#42568,#9977);
#7109=LINE('',#42605,#9978);
#7110=LINE('',#42642,#9979);
#7111=LINE('',#42680,#9980);
#7112=LINE('',#42717,#9981);
#7113=LINE('',#42754,#9982);
#7114=LINE('',#42785,#9983);
#7115=LINE('',#42809,#9984);
#7116=LINE('',#42837,#9985);
#7117=LINE('',#42874,#9986);
#7118=LINE('',#42911,#9987);
#7119=LINE('',#42948,#9988);
#7120=LINE('',#42986,#9989);
#7121=LINE('',#43023,#9990);
#7122=LINE('',#43060,#9991);
#7123=LINE('',#43098,#9992);
#7124=LINE('',#45572,#9993);
#7125=LINE('',#45574,#9994);
#7126=LINE('',#45576,#9995);
#7127=LINE('',#45577,#9996);
#7128=LINE('',#45581,#9997);
#7129=LINE('',#45584,#9998);
#7130=LINE('',#45585,#9999);
#7131=LINE('',#45591,#10000);
#7132=LINE('',#45593,#10001);
#7133=LINE('',#45595,#10002);
#7134=LINE('',#45596,#10003);
#7135=LINE('',#45600,#10004);
#7136=LINE('',#45603,#10005);
#7137=LINE('',#45604,#10006);
#7138=LINE('',#45610,#10007);
#7139=LINE('',#45612,#10008);
#7140=LINE('',#45614,#10009);
#7141=LINE('',#45615,#10010);
#7142=LINE('',#45619,#10011);
#7143=LINE('',#45622,#10012);
#7144=LINE('',#45623,#10013);
#7145=LINE('',#45629,#10014);
#7146=LINE('',#45631,#10015);
#7147=LINE('',#45633,#10016);
#7148=LINE('',#45634,#10017);
#7149=LINE('',#45638,#10018);
#7150=LINE('',#45641,#10019);
#7151=LINE('',#45642,#10020);
#7152=LINE('',#45648,#10021);
#7153=LINE('',#45650,#10022);
#7154=LINE('',#45652,#10023);
#7155=LINE('',#45653,#10024);
#7156=LINE('',#45657,#10025);
#7157=LINE('',#45660,#10026);
#7158=LINE('',#45661,#10027);
#7159=LINE('',#45667,#10028);
#7160=LINE('',#45669,#10029);
#7161=LINE('',#45671,#10030);
#7162=LINE('',#45672,#10031);
#7163=LINE('',#45676,#10032);
#7164=LINE('',#45679,#10033);
#7165=LINE('',#45680,#10034);
#7166=LINE('',#45686,#10035);
#7167=LINE('',#45688,#10036);
#7168=LINE('',#45690,#10037);
#7169=LINE('',#45691,#10038);
#7170=LINE('',#45695,#10039);
#7171=LINE('',#45698,#10040);
#7172=LINE('',#45699,#10041);
#7173=LINE('',#45705,#10042);
#7174=LINE('',#45707,#10043);
#7175=LINE('',#45709,#10044);
#7176=LINE('',#45710,#10045);
#7177=LINE('',#45714,#10046);
#7178=LINE('',#45717,#10047);
#7179=LINE('',#45718,#10048);
#7180=LINE('',#45724,#10049);
#7181=LINE('',#45726,#10050);
#7182=LINE('',#45728,#10051);
#7183=LINE('',#45729,#10052);
#7184=LINE('',#45733,#10053);
#7185=LINE('',#45736,#10054);
#7186=LINE('',#45737,#10055);
#7187=LINE('',#45743,#10056);
#7188=LINE('',#45745,#10057);
#7189=LINE('',#45747,#10058);
#7190=LINE('',#45748,#10059);
#7191=LINE('',#45752,#10060);
#7192=LINE('',#45755,#10061);
#7193=LINE('',#45756,#10062);
#7194=LINE('',#45762,#10063);
#7195=LINE('',#45764,#10064);
#7196=LINE('',#45766,#10065);
#7197=LINE('',#45767,#10066);
#7198=LINE('',#45771,#10067);
#7199=LINE('',#45774,#10068);
#7200=LINE('',#45775,#10069);
#7201=LINE('',#45781,#10070);
#7202=LINE('',#45783,#10071);
#7203=LINE('',#45785,#10072);
#7204=LINE('',#45786,#10073);
#7205=LINE('',#45790,#10074);
#7206=LINE('',#45793,#10075);
#7207=LINE('',#45794,#10076);
#7208=LINE('',#45800,#10077);
#7209=LINE('',#45802,#10078);
#7210=LINE('',#45804,#10079);
#7211=LINE('',#45805,#10080);
#7212=LINE('',#45809,#10081);
#7213=LINE('',#45812,#10082);
#7214=LINE('',#45813,#10083);
#7215=LINE('',#45819,#10084);
#7216=LINE('',#45821,#10085);
#7217=LINE('',#45823,#10086);
#7218=LINE('',#45824,#10087);
#7219=LINE('',#45828,#10088);
#7220=LINE('',#45831,#10089);
#7221=LINE('',#45832,#10090);
#7222=LINE('',#45838,#10091);
#7223=LINE('',#45840,#10092);
#7224=LINE('',#45842,#10093);
#7225=LINE('',#45843,#10094);
#7226=LINE('',#45847,#10095);
#7227=LINE('',#45850,#10096);
#7228=LINE('',#45851,#10097);
#7229=LINE('',#45857,#10098);
#7230=LINE('',#45859,#10099);
#7231=LINE('',#45861,#10100);
#7232=LINE('',#45862,#10101);
#7233=LINE('',#45866,#10102);
#7234=LINE('',#45869,#10103);
#7235=LINE('',#45870,#10104);
#7236=LINE('',#45876,#10105);
#7237=LINE('',#45878,#10106);
#7238=LINE('',#45880,#10107);
#7239=LINE('',#45881,#10108);
#7240=LINE('',#45885,#10109);
#7241=LINE('',#45888,#10110);
#7242=LINE('',#45889,#10111);
#7243=LINE('',#45895,#10112);
#7244=LINE('',#45897,#10113);
#7245=LINE('',#45899,#10114);
#7246=LINE('',#45900,#10115);
#7247=LINE('',#45905,#10116);
#7248=LINE('',#45909,#10117);
#7249=LINE('',#45910,#10118);
#7250=LINE('',#45918,#10119);
#7251=LINE('',#45920,#10120);
#7252=LINE('',#45922,#10121);
#7253=LINE('',#45923,#10122);
#7254=LINE('',#45927,#10123);
#7255=LINE('',#45930,#10124);
#7256=LINE('',#45931,#10125);
#7257=LINE('',#45937,#10126);
#7258=LINE('',#45939,#10127);
#7259=LINE('',#45941,#10128);
#7260=LINE('',#45942,#10129);
#7261=LINE('',#45946,#10130);
#7262=LINE('',#45949,#10131);
#7263=LINE('',#45950,#10132);
#7264=LINE('',#45956,#10133);
#7265=LINE('',#45958,#10134);
#7266=LINE('',#45960,#10135);
#7267=LINE('',#45961,#10136);
#7268=LINE('',#45965,#10137);
#7269=LINE('',#45968,#10138);
#7270=LINE('',#45969,#10139);
#7271=LINE('',#45975,#10140);
#7272=LINE('',#45977,#10141);
#7273=LINE('',#45979,#10142);
#7274=LINE('',#45980,#10143);
#7275=LINE('',#45984,#10144);
#7276=LINE('',#45987,#10145);
#7277=LINE('',#45988,#10146);
#7278=LINE('',#45994,#10147);
#7279=LINE('',#45996,#10148);
#7280=LINE('',#45998,#10149);
#7281=LINE('',#45999,#10150);
#7282=LINE('',#46003,#10151);
#7283=LINE('',#46006,#10152);
#7284=LINE('',#46007,#10153);
#7285=LINE('',#46013,#10154);
#7286=LINE('',#46015,#10155);
#7287=LINE('',#46017,#10156);
#7288=LINE('',#46018,#10157);
#7289=LINE('',#46022,#10158);
#7290=LINE('',#46025,#10159);
#7291=LINE('',#46026,#10160);
#7292=LINE('',#46032,#10161);
#7293=LINE('',#46034,#10162);
#7294=LINE('',#46036,#10163);
#7295=LINE('',#46037,#10164);
#7296=LINE('',#46041,#10165);
#7297=LINE('',#46044,#10166);
#7298=LINE('',#46045,#10167);
#7299=LINE('',#46051,#10168);
#7300=LINE('',#46053,#10169);
#7301=LINE('',#46055,#10170);
#7302=LINE('',#46056,#10171);
#7303=LINE('',#46060,#10172);
#7304=LINE('',#46063,#10173);
#7305=LINE('',#46064,#10174);
#7306=LINE('',#46070,#10175);
#7307=LINE('',#46072,#10176);
#7308=LINE('',#46074,#10177);
#7309=LINE('',#46075,#10178);
#7310=LINE('',#46079,#10179);
#7311=LINE('',#46082,#10180);
#7312=LINE('',#46083,#10181);
#7313=LINE('',#46089,#10182);
#7314=LINE('',#46091,#10183);
#7315=LINE('',#46093,#10184);
#7316=LINE('',#46094,#10185);
#7317=LINE('',#46098,#10186);
#7318=LINE('',#46101,#10187);
#7319=LINE('',#46102,#10188);
#7320=LINE('',#46108,#10189);
#7321=LINE('',#46110,#10190);
#7322=LINE('',#46112,#10191);
#7323=LINE('',#46113,#10192);
#7324=LINE('',#46117,#10193);
#7325=LINE('',#46120,#10194);
#7326=LINE('',#46121,#10195);
#7327=LINE('',#46127,#10196);
#7328=LINE('',#46129,#10197);
#7329=LINE('',#46131,#10198);
#7330=LINE('',#46132,#10199);
#7331=LINE('',#46136,#10200);
#7332=LINE('',#46139,#10201);
#7333=LINE('',#46140,#10202);
#7334=LINE('',#46146,#10203);
#7335=LINE('',#46148,#10204);
#7336=LINE('',#46150,#10205);
#7337=LINE('',#46151,#10206);
#7338=LINE('',#46155,#10207);
#7339=LINE('',#46158,#10208);
#7340=LINE('',#46159,#10209);
#7341=LINE('',#46165,#10210);
#7342=LINE('',#46167,#10211);
#7343=LINE('',#46169,#10212);
#7344=LINE('',#46170,#10213);
#7345=LINE('',#46174,#10214);
#7346=LINE('',#46177,#10215);
#7347=LINE('',#46178,#10216);
#7348=LINE('',#46184,#10217);
#7349=LINE('',#46186,#10218);
#7350=LINE('',#46188,#10219);
#7351=LINE('',#46189,#10220);
#7352=LINE('',#46193,#10221);
#7353=LINE('',#46196,#10222);
#7354=LINE('',#46197,#10223);
#7355=LINE('',#46203,#10224);
#7356=LINE('',#46205,#10225);
#7357=LINE('',#46207,#10226);
#7358=LINE('',#46208,#10227);
#7359=LINE('',#46212,#10228);
#7360=LINE('',#46215,#10229);
#7361=LINE('',#46216,#10230);
#7362=LINE('',#46222,#10231);
#7363=LINE('',#46224,#10232);
#7364=LINE('',#46226,#10233);
#7365=LINE('',#46227,#10234);
#7366=LINE('',#46231,#10235);
#7367=LINE('',#46234,#10236);
#7368=LINE('',#46235,#10237);
#7369=LINE('',#46241,#10238);
#7370=LINE('',#46243,#10239);
#7371=LINE('',#46245,#10240);
#7372=LINE('',#46246,#10241);
#7373=LINE('',#46250,#10242);
#7374=LINE('',#46253,#10243);
#7375=LINE('',#46254,#10244);
#7376=LINE('',#46260,#10245);
#7377=LINE('',#46262,#10246);
#7378=LINE('',#46264,#10247);
#7379=LINE('',#46265,#10248);
#7380=LINE('',#46268,#10249);
#7381=LINE('',#46270,#10250);
#7382=LINE('',#46271,#10251);
#7383=LINE('',#46274,#10252);
#7384=LINE('',#46276,#10253);
#7385=LINE('',#46277,#10254);
#7386=LINE('',#46280,#10255);
#7387=LINE('',#46282,#10256);
#7388=LINE('',#46283,#10257);
#7389=LINE('',#46286,#10258);
#7390=LINE('',#46288,#10259);
#7391=LINE('',#46289,#10260);
#7392=LINE('',#46291,#10261);
#7393=LINE('',#46292,#10262);
#7394=LINE('',#46298,#10263);
#7395=LINE('',#46304,#10264);
#7396=LINE('',#46308,#10265);
#7397=LINE('',#46315,#10266);
#7398=LINE('',#46316,#10267);
#7399=LINE('',#46320,#10268);
#7400=LINE('',#46329,#10269);
#7401=LINE('',#46333,#10270);
#7402=LINE('',#46337,#10271);
#7403=VECTOR('',#26941,8.75);
#7404=VECTOR('',#26950,9.);
#7405=VECTOR('',#26957,8.75);
#7406=VECTOR('',#26966,9.);
#7407=VECTOR('',#26973,10.25);
#7408=VECTOR('',#26980,10.);
#7409=VECTOR('',#26991,10.25);
#7410=VECTOR('',#26994,10.);
#7411=VECTOR('',#26997,10.);
#7412=VECTOR('',#27000,10.);
#7413=VECTOR('',#27001,10.);
#7414=VECTOR('',#27004,10.);
#7415=VECTOR('',#27005,10.);
#7416=VECTOR('',#27006,10.);
#7417=VECTOR('',#27009,10.);
#7418=VECTOR('',#27012,10.);
#7419=VECTOR('',#27015,10.);
#7420=VECTOR('',#27018,10.);
#7421=VECTOR('',#27021,10.);
#7422=VECTOR('',#27026,10.);
#7423=VECTOR('',#27027,10.);
#7424=VECTOR('',#27028,10.);
#7425=VECTOR('',#27031,10.);
#7426=VECTOR('',#27032,10.);
#7427=VECTOR('',#27033,10.);
#7428=VECTOR('',#27038,10.);
#7429=VECTOR('',#27041,10.);
#7430=VECTOR('',#27044,10.);
#7431=VECTOR('',#27049,10.);
#7432=VECTOR('',#27050,10.);
#7433=VECTOR('',#27051,10.);
#7434=VECTOR('',#27052,10.);
#7435=VECTOR('',#27053,10.);
#7436=VECTOR('',#27056,10.);
#7437=VECTOR('',#27059,10.);
#7438=VECTOR('',#27064,10.);
#7439=VECTOR('',#27077,10.);
#7440=VECTOR('',#27082,10.);
#7441=VECTOR('',#27087,10.);
#7442=VECTOR('',#27090,10.);
#7443=VECTOR('',#27091,10.);
#7444=VECTOR('',#27092,10.);
#7445=VECTOR('',#27095,10.);
#7446=VECTOR('',#27096,10.);
#7447=VECTOR('',#27099,10.);
#7448=VECTOR('',#27102,10.);
#7449=VECTOR('',#27103,10.);
#7450=VECTOR('',#27106,5.3);
#7451=VECTOR('',#27113,5.05);
#7452=VECTOR('',#27116,5.3);
#7453=VECTOR('',#27123,5.05);
#7454=VECTOR('',#27126,10.);
#7455=VECTOR('',#27127,10.);
#7456=VECTOR('',#27132,5.05);
#7457=VECTOR('',#27137,10.);
#7458=VECTOR('',#27142,10.);
#7459=VECTOR('',#27143,10.);
#7460=VECTOR('',#27148,5.05);
#7461=VECTOR('',#27153,10.);
#7462=VECTOR('',#27158,10.);
#7463=VECTOR('',#27161,10.);
#7464=VECTOR('',#27166,5.3);
#7465=VECTOR('',#27171,10.);
#7466=VECTOR('',#27174,10.);
#7467=VECTOR('',#27177,10.);
#7468=VECTOR('',#27180,10.);
#7469=VECTOR('',#27187,10.);
#7470=VECTOR('',#27190,10.);
#7471=VECTOR('',#27203,5.3);
#7472=VECTOR('',#27206,5.3);
#7473=VECTOR('',#27209,5.3);
#7474=VECTOR('',#27212,5.75);
#7475=VECTOR('',#27219,5.5);
#7476=VECTOR('',#27222,5.75);
#7477=VECTOR('',#27229,5.5);
#7478=VECTOR('',#27230,10.);
#7479=VECTOR('',#27233,10.);
#7480=VECTOR('',#27234,10.);
#7481=VECTOR('',#27235,10.);
#7482=VECTOR('',#27238,10.);
#7483=VECTOR('',#27241,10.);
#7484=VECTOR('',#27242,10.);
#7485=VECTOR('',#27243,10.);
#7486=VECTOR('',#27246,10.);
#7487=VECTOR('',#27247,10.);
#7488=VECTOR('',#27250,10.);
#7489=VECTOR('',#27253,10.);
#7490=VECTOR('',#27254,10.);
#7491=VECTOR('',#27257,5.75);
#7492=VECTOR('',#27260,5.75);
#7493=VECTOR('',#27263,10.);
#7494=VECTOR('',#27264,10.);
#7495=VECTOR('',#27265,10.);
#7496=VECTOR('',#27266,10.);
#7497=VECTOR('',#27269,10.);
#7498=VECTOR('',#27276,10.);
#7499=VECTOR('',#27277,10.);
#7500=VECTOR('',#27280,10.);
#7501=VECTOR('',#27287,10.);
#7502=VECTOR('',#27288,10.);
#7503=VECTOR('',#27289,10.);
#7504=VECTOR('',#27292,10.);
#7505=VECTOR('',#27301,10.);
#7506=VECTOR('',#27304,10.);
#7507=VECTOR('',#27323,10.);
#7508=VECTOR('',#27326,10.);
#7509=VECTOR('',#27329,10.);
#7510=VECTOR('',#27332,10.);
#7511=VECTOR('',#27335,10.);
#7512=VECTOR('',#27336,10.);
#7513=VECTOR('',#27339,10.);
#7514=VECTOR('',#27360,10.);
#7515=VECTOR('',#27363,10.);
#7516=VECTOR('',#27366,10.);
#7517=VECTOR('',#27369,10.);
#7518=VECTOR('',#27372,10.);
#7519=VECTOR('',#27373,10.);
#7520=VECTOR('',#27376,10.);
#7521=VECTOR('',#27389,10.);
#7522=VECTOR('',#27396,10.);
#7523=VECTOR('',#27399,10.);
#7524=VECTOR('',#27402,10.);
#7525=VECTOR('',#27423,10.);
#7526=VECTOR('',#27432,10.);
#7527=VECTOR('',#27435,10.);
#7528=VECTOR('',#27436,10.);
#7529=VECTOR('',#27439,10.);
#7530=VECTOR('',#27444,10.);
#7531=VECTOR('',#27445,10.);
#7532=VECTOR('',#27448,10.);
#7533=VECTOR('',#27453,10.);
#7534=VECTOR('',#27454,10.);
#7535=VECTOR('',#27457,10.);
#7536=VECTOR('',#27462,10.);
#7537=VECTOR('',#27469,10.);
#7538=VECTOR('',#27482,10.);
#7539=VECTOR('',#27493,10.);
#7540=VECTOR('',#27502,10.);
#7541=VECTOR('',#27511,10.);
#7542=VECTOR('',#27514,10.);
#7543=VECTOR('',#27517,10.);
#7544=VECTOR('',#27520,10.);
#7545=VECTOR('',#27521,10.);
#7546=VECTOR('',#27524,10.);
#7547=VECTOR('',#27529,10.);
#7548=VECTOR('',#27530,10.);
#7549=VECTOR('',#27533,10.);
#7550=VECTOR('',#27538,10.);
#7551=VECTOR('',#27541,10.);
#7552=VECTOR('',#27544,10.);
#7553=VECTOR('',#27547,10.);
#7554=VECTOR('',#27554,10.);
#7555=VECTOR('',#27563,10.);
#7556=VECTOR('',#27566,10.);
#7557=VECTOR('',#27567,10.);
#7558=VECTOR('',#27598,10.);
#7559=VECTOR('',#27607,10.);
#7560=VECTOR('',#27622,41.28);
#7561=VECTOR('',#27629,10.);
#7562=VECTOR('',#27632,10.);
#7563=VECTOR('',#27653,10.);
#7564=VECTOR('',#27666,10.);
#7565=VECTOR('',#27673,10.);
#7566=VECTOR('',#27676,10.);
#7567=VECTOR('',#27679,10.);
#7568=VECTOR('',#27680,10.);
#7569=VECTOR('',#27685,10.);
#7570=VECTOR('',#27698,10.);
#7571=VECTOR('',#27705,10.);
#7572=VECTOR('',#27708,10.);
#7573=VECTOR('',#27711,10.);
#7574=VECTOR('',#27712,10.);
#7575=VECTOR('',#27715,10.);
#7576=VECTOR('',#27720,10.);
#7577=VECTOR('',#27723,10.);
#7578=VECTOR('',#27728,10.);
#7579=VECTOR('',#27733,4.01);
#7580=VECTOR('',#27740,4.01);
#7581=VECTOR('',#27753,14.7);
#7582=VECTOR('',#27762,14.3);
#7583=VECTOR('',#27765,14.3);
#7584=VECTOR('',#27772,10.);
#7585=VECTOR('',#27777,10.);
#7586=VECTOR('',#27780,10.);
#7587=VECTOR('',#27783,10.);
#7588=VECTOR('',#27786,10.);
#7589=VECTOR('',#27789,10.);
#7590=VECTOR('',#27796,10.);
#7591=VECTOR('',#27805,13.8);
#7592=VECTOR('',#27810,13.55);
#7593=VECTOR('',#27821,13.8);
#7594=VECTOR('',#27826,13.55);
#7595=VECTOR('',#27837,10.);
#7596=VECTOR('',#27840,10.);
#7597=VECTOR('',#27853,10.);
#7598=VECTOR('',#27854,10.);
#7599=VECTOR('',#27867,10.);
#7600=VECTOR('',#27868,10.);
#7601=VECTOR('',#27881,10.);
#7602=VECTOR('',#27882,10.);
#7603=VECTOR('',#27891,10.);
#7604=VECTOR('',#27894,10.);
#7605=VECTOR('',#27897,10.);
#7606=VECTOR('',#27898,10.);
#7607=VECTOR('',#27901,10.);
#7608=VECTOR('',#27906,10.);
#7609=VECTOR('',#27907,10.);
#7610=VECTOR('',#27934,10.);
#7611=VECTOR('',#27947,10.);
#7612=VECTOR('',#27948,10.);
#7613=VECTOR('',#27961,10.);
#7614=VECTOR('',#27962,10.);
#7615=VECTOR('',#27973,10.);
#7616=VECTOR('',#27980,10.);
#7617=VECTOR('',#27981,10.);
#7618=VECTOR('',#27984,10.);
#7619=VECTOR('',#28007,4.01);
#7620=VECTOR('',#28014,4.01);
#7621=VECTOR('',#28021,4.01);
#7622=VECTOR('',#28028,4.01);
#7623=VECTOR('',#28035,5.3);
#7624=VECTOR('',#28038,5.3);
#7625=VECTOR('',#28041,5.3);
#7626=VECTOR('',#28044,5.3);
#7627=VECTOR('',#28049,8.);
#7628=VECTOR('',#28052,10.);
#7629=VECTOR('',#28053,10.);
#7630=VECTOR('',#28054,10.);
#7631=VECTOR('',#28055,10.);
#7632=VECTOR('',#28062,21.);
#7633=VECTOR('',#28067,8.);
#7634=VECTOR('',#28074,21.);
#7635=VECTOR('',#28083,7.45);
#7636=VECTOR('',#28092,7.2);
#7637=VECTOR('',#28097,10.);
#7638=VECTOR('',#28098,10.);
#7639=VECTOR('',#28099,10.);
#7640=VECTOR('',#28100,10.);
#7641=VECTOR('',#28103,10.);
#7642=VECTOR('',#28110,10.);
#7643=VECTOR('',#28111,10.);
#7644=VECTOR('',#28112,10.);
#7645=VECTOR('',#28121,10.);
#7646=VECTOR('',#28124,10.);
#7647=VECTOR('',#28127,10.);
#7648=VECTOR('',#28128,10.);
#7649=VECTOR('',#28133,10.);
#7650=VECTOR('',#28136,10.);
#7651=VECTOR('',#28139,10.);
#7652=VECTOR('',#28142,10.);
#7653=VECTOR('',#28157,10.);
#7654=VECTOR('',#28158,10.);
#7655=VECTOR('',#28159,10.);
#7656=VECTOR('',#28160,10.);
#7657=VECTOR('',#28163,10.);
#7658=VECTOR('',#28170,10.);
#7659=VECTOR('',#28171,10.);
#7660=VECTOR('',#28172,10.);
#7661=VECTOR('',#28181,10.);
#7662=VECTOR('',#28184,10.);
#7663=VECTOR('',#28187,10.);
#7664=VECTOR('',#28188,10.);
#7665=VECTOR('',#28193,8.75);
#7666=VECTOR('',#28200,10.);
#7667=VECTOR('',#28201,10.);
#7668=VECTOR('',#28202,10.);
#7669=VECTOR('',#28203,10.);
#7670=VECTOR('',#28204,10.);
#7671=VECTOR('',#28205,10.);
#7672=VECTOR('',#28208,8.5);
#7673=VECTOR('',#28213,8.75);
#7674=VECTOR('',#28220,8.5);
#7675=VECTOR('',#28225,8.75);
#7676=VECTOR('',#28234,10.);
#7677=VECTOR('',#28235,10.);
#7678=VECTOR('',#28236,10.);
#7679=VECTOR('',#28237,10.);
#7680=VECTOR('',#28238,10.);
#7681=VECTOR('',#28239,10.);
#7682=VECTOR('',#28242,8.5);
#7683=VECTOR('',#28247,8.75);
#7684=VECTOR('',#28256,8.5);
#7685=VECTOR('',#28261,10.);
#7686=VECTOR('',#28264,10.);
#7687=VECTOR('',#28267,10.);
#7688=VECTOR('',#28268,10.);
#7689=VECTOR('',#28271,10.);
#7690=VECTOR('',#28276,10.);
#7691=VECTOR('',#28277,10.);
#7692=VECTOR('',#28280,10.);
#7693=VECTOR('',#28285,10.);
#7694=VECTOR('',#28286,10.);
#7695=VECTOR('',#28289,10.);
#7696=VECTOR('',#28294,10.);
#7697=VECTOR('',#28297,10.);
#7698=VECTOR('',#28298,10.);
#7699=VECTOR('',#28299,10.);
#7700=VECTOR('',#28302,10.);
#7701=VECTOR('',#28307,10.);
#7702=VECTOR('',#28308,10.);
#7703=VECTOR('',#28311,10.);
#7704=VECTOR('',#28316,10.);
#7705=VECTOR('',#28317,10.);
#7706=VECTOR('',#28320,10.);
#7707=VECTOR('',#28325,10.);
#7708=VECTOR('',#28326,10.);
#7709=VECTOR('',#28329,10.);
#7710=VECTOR('',#28334,10.);
#7711=VECTOR('',#28335,10.);
#7712=VECTOR('',#28338,10.);
#7713=VECTOR('',#28345,10.);
#7714=VECTOR('',#28346,10.);
#7715=VECTOR('',#28347,10.);
#7716=VECTOR('',#28356,10.);
#7717=VECTOR('',#28361,10.);
#7718=VECTOR('',#28362,10.);
#7719=VECTOR('',#28369,10.);
#7720=VECTOR('',#28374,10.);
#7721=VECTOR('',#28375,10.);
#7722=VECTOR('',#28386,10.);
#7723=VECTOR('',#28391,10.);
#7724=VECTOR('',#28394,10.);
#7725=VECTOR('',#28399,10.);
#7726=VECTOR('',#28404,11.);
#7727=VECTOR('',#28409,4.01);
#7728=VECTOR('',#28416,4.01);
#7729=VECTOR('',#28425,5.3);
#7730=VECTOR('',#28430,5.3);
#7731=VECTOR('',#28435,5.3);
#7732=VECTOR('',#28440,5.3);
#7733=VECTOR('',#28451,10.);
#7734=VECTOR('',#28454,10.);
#7735=VECTOR('',#28457,10.);
#7736=VECTOR('',#28464,10.);
#7737=VECTOR('',#28465,10.);
#7738=VECTOR('',#28466,10.);
#7739=VECTOR('',#28467,10.);
#7740=VECTOR('',#28468,10.);
#7741=VECTOR('',#28469,10.);
#7742=VECTOR('',#28472,10.);
#7743=VECTOR('',#28473,10.);
#7744=VECTOR('',#28474,10.);
#7745=VECTOR('',#28475,10.);
#7746=VECTOR('',#28476,10.);
#7747=VECTOR('',#28477,10.);
#7748=VECTOR('',#28478,10.);
#7749=VECTOR('',#28479,10.);
#7750=VECTOR('',#28480,10.);
#7751=VECTOR('',#28481,10.);
#7752=VECTOR('',#28482,10.);
#7753=VECTOR('',#28483,10.);
#7754=VECTOR('',#28484,10.);
#7755=VECTOR('',#28485,10.);
#7756=VECTOR('',#28486,10.);
#7757=VECTOR('',#28487,10.);
#7758=VECTOR('',#28488,10.);
#7759=VECTOR('',#28489,10.);
#7760=VECTOR('',#28490,10.);
#7761=VECTOR('',#28491,10.);
#7762=VECTOR('',#28492,10.);
#7763=VECTOR('',#28493,10.);
#7764=VECTOR('',#28494,10.);
#7765=VECTOR('',#28495,10.);
#7766=VECTOR('',#28496,10.);
#7767=VECTOR('',#28497,10.);
#7768=VECTOR('',#28498,10.);
#7769=VECTOR('',#28499,10.);
#7770=VECTOR('',#28500,10.);
#7771=VECTOR('',#28501,10.);
#7772=VECTOR('',#28502,10.);
#7773=VECTOR('',#28503,10.);
#7774=VECTOR('',#28504,10.);
#7775=VECTOR('',#28505,10.);
#7776=VECTOR('',#28506,10.);
#7777=VECTOR('',#28507,10.);
#7778=VECTOR('',#28508,10.);
#7779=VECTOR('',#28509,10.);
#7780=VECTOR('',#28510,10.);
#7781=VECTOR('',#28511,10.);
#7782=VECTOR('',#28512,10.);
#7783=VECTOR('',#28513,10.);
#7784=VECTOR('',#28514,10.);
#7785=VECTOR('',#28515,10.);
#7786=VECTOR('',#28516,10.);
#7787=VECTOR('',#28517,10.);
#7788=VECTOR('',#28518,10.);
#7789=VECTOR('',#28519,10.);
#7790=VECTOR('',#28520,10.);
#7791=VECTOR('',#28521,10.);
#7792=VECTOR('',#28522,10.);
#7793=VECTOR('',#28523,10.);
#7794=VECTOR('',#28524,10.);
#7795=VECTOR('',#28525,10.);
#7796=VECTOR('',#28526,10.);
#7797=VECTOR('',#28527,10.);
#7798=VECTOR('',#28528,10.);
#7799=VECTOR('',#28529,10.);
#7800=VECTOR('',#28530,10.);
#7801=VECTOR('',#28531,10.);
#7802=VECTOR('',#28532,10.);
#7803=VECTOR('',#28533,10.);
#7804=VECTOR('',#28534,10.);
#7805=VECTOR('',#28535,10.);
#7806=VECTOR('',#28536,10.);
#7807=VECTOR('',#28537,10.);
#7808=VECTOR('',#28538,10.);
#7809=VECTOR('',#28539,10.);
#7810=VECTOR('',#28540,10.);
#7811=VECTOR('',#28541,10.);
#7812=VECTOR('',#28542,10.);
#7813=VECTOR('',#28543,10.);
#7814=VECTOR('',#28544,10.);
#7815=VECTOR('',#28545,10.);
#7816=VECTOR('',#28546,10.);
#7817=VECTOR('',#28547,10.);
#7818=VECTOR('',#28548,10.);
#7819=VECTOR('',#28549,10.);
#7820=VECTOR('',#28550,10.);
#7821=VECTOR('',#28551,10.);
#7822=VECTOR('',#28552,10.);
#7823=VECTOR('',#28553,10.);
#7824=VECTOR('',#28554,10.);
#7825=VECTOR('',#28555,10.);
#7826=VECTOR('',#28556,10.);
#7827=VECTOR('',#28557,10.);
#7828=VECTOR('',#28558,10.);
#7829=VECTOR('',#28559,10.);
#7830=VECTOR('',#28560,10.);
#7831=VECTOR('',#28561,10.);
#7832=VECTOR('',#28562,10.);
#7833=VECTOR('',#28563,10.);
#7834=VECTOR('',#28564,10.);
#7835=VECTOR('',#28565,10.);
#7836=VECTOR('',#28566,10.);
#7837=VECTOR('',#28567,10.);
#7838=VECTOR('',#28568,10.);
#7839=VECTOR('',#28569,10.);
#7840=VECTOR('',#28570,10.);
#7841=VECTOR('',#28571,10.);
#7842=VECTOR('',#28572,10.);
#7843=VECTOR('',#28573,10.);
#7844=VECTOR('',#28574,10.);
#7845=VECTOR('',#28575,10.);
#7846=VECTOR('',#28576,10.);
#7847=VECTOR('',#28577,10.);
#7848=VECTOR('',#28578,10.);
#7849=VECTOR('',#28579,10.);
#7850=VECTOR('',#28580,10.);
#7851=VECTOR('',#28581,10.);
#7852=VECTOR('',#28582,10.);
#7853=VECTOR('',#28583,10.);
#7854=VECTOR('',#28584,10.);
#7855=VECTOR('',#28585,10.);
#7856=VECTOR('',#28586,10.);
#7857=VECTOR('',#28587,10.);
#7858=VECTOR('',#28588,10.);
#7859=VECTOR('',#28589,10.);
#7860=VECTOR('',#28590,10.);
#7861=VECTOR('',#28591,10.);
#7862=VECTOR('',#28592,10.);
#7863=VECTOR('',#28593,10.);
#7864=VECTOR('',#28594,10.);
#7865=VECTOR('',#28595,10.);
#7866=VECTOR('',#28596,10.);
#7867=VECTOR('',#28597,10.);
#7868=VECTOR('',#28598,10.);
#7869=VECTOR('',#28599,10.);
#7870=VECTOR('',#28600,10.);
#7871=VECTOR('',#28601,10.);
#7872=VECTOR('',#28602,10.);
#7873=VECTOR('',#28603,10.);
#7874=VECTOR('',#28604,10.);
#7875=VECTOR('',#28605,10.);
#7876=VECTOR('',#28606,10.);
#7877=VECTOR('',#28607,10.);
#7878=VECTOR('',#28608,10.);
#7879=VECTOR('',#28609,10.);
#7880=VECTOR('',#28610,10.);
#7881=VECTOR('',#28611,10.);
#7882=VECTOR('',#28612,10.);
#7883=VECTOR('',#28613,10.);
#7884=VECTOR('',#28614,10.);
#7885=VECTOR('',#28615,10.);
#7886=VECTOR('',#28616,10.);
#7887=VECTOR('',#28617,10.);
#7888=VECTOR('',#28618,10.);
#7889=VECTOR('',#28619,10.);
#7890=VECTOR('',#28620,10.);
#7891=VECTOR('',#28621,10.);
#7892=VECTOR('',#28622,10.);
#7893=VECTOR('',#28623,10.);
#7894=VECTOR('',#28624,10.);
#7895=VECTOR('',#28625,10.);
#7896=VECTOR('',#28626,10.);
#7897=VECTOR('',#28627,10.);
#7898=VECTOR('',#28628,10.);
#7899=VECTOR('',#28629,10.);
#7900=VECTOR('',#28630,10.);
#7901=VECTOR('',#28631,10.);
#7902=VECTOR('',#28632,10.);
#7903=VECTOR('',#28633,10.);
#7904=VECTOR('',#28634,10.);
#7905=VECTOR('',#28635,10.);
#7906=VECTOR('',#28636,10.);
#7907=VECTOR('',#28637,10.);
#7908=VECTOR('',#28638,10.);
#7909=VECTOR('',#28639,10.);
#7910=VECTOR('',#28640,10.);
#7911=VECTOR('',#28641,10.);
#7912=VECTOR('',#28642,10.);
#7913=VECTOR('',#28643,10.);
#7914=VECTOR('',#28644,10.);
#7915=VECTOR('',#28645,10.);
#7916=VECTOR('',#28646,10.);
#7917=VECTOR('',#28647,10.);
#7918=VECTOR('',#28648,10.);
#7919=VECTOR('',#28649,10.);
#7920=VECTOR('',#28650,10.);
#7921=VECTOR('',#28651,10.);
#7922=VECTOR('',#28652,10.);
#7923=VECTOR('',#28653,10.);
#7924=VECTOR('',#28654,10.);
#7925=VECTOR('',#28655,10.);
#7926=VECTOR('',#28656,10.);
#7927=VECTOR('',#28657,10.);
#7928=VECTOR('',#28658,10.);
#7929=VECTOR('',#28659,10.);
#7930=VECTOR('',#28660,10.);
#7931=VECTOR('',#28661,10.);
#7932=VECTOR('',#28662,10.);
#7933=VECTOR('',#28663,10.);
#7934=VECTOR('',#28664,10.);
#7935=VECTOR('',#28665,10.);
#7936=VECTOR('',#28666,10.);
#7937=VECTOR('',#28667,10.);
#7938=VECTOR('',#28668,10.);
#7939=VECTOR('',#28669,10.);
#7940=VECTOR('',#28670,10.);
#7941=VECTOR('',#28671,10.);
#7942=VECTOR('',#28672,10.);
#7943=VECTOR('',#28673,10.);
#7944=VECTOR('',#28674,10.);
#7945=VECTOR('',#28675,10.);
#7946=VECTOR('',#28676,10.);
#7947=VECTOR('',#28677,10.);
#7948=VECTOR('',#28678,10.);
#7949=VECTOR('',#28679,10.);
#7950=VECTOR('',#28680,10.);
#7951=VECTOR('',#28681,10.);
#7952=VECTOR('',#28682,10.);
#7953=VECTOR('',#28683,10.);
#7954=VECTOR('',#28684,10.);
#7955=VECTOR('',#28685,10.);
#7956=VECTOR('',#28686,10.);
#7957=VECTOR('',#28687,10.);
#7958=VECTOR('',#28688,10.);
#7959=VECTOR('',#28689,10.);
#7960=VECTOR('',#28690,10.);
#7961=VECTOR('',#28691,10.);
#7962=VECTOR('',#28692,10.);
#7963=VECTOR('',#28693,10.);
#7964=VECTOR('',#28694,10.);
#7965=VECTOR('',#28695,10.);
#7966=VECTOR('',#28696,10.);
#7967=VECTOR('',#28697,10.);
#7968=VECTOR('',#28698,10.);
#7969=VECTOR('',#28699,10.);
#7970=VECTOR('',#28700,10.);
#7971=VECTOR('',#28701,10.);
#7972=VECTOR('',#28702,10.);
#7973=VECTOR('',#28703,10.);
#7974=VECTOR('',#28704,10.);
#7975=VECTOR('',#28705,10.);
#7976=VECTOR('',#28706,10.);
#7977=VECTOR('',#28707,10.);
#7978=VECTOR('',#28708,10.);
#7979=VECTOR('',#28709,10.);
#7980=VECTOR('',#28710,10.);
#7981=VECTOR('',#28715,10.);
#7982=VECTOR('',#28716,10.);
#7983=VECTOR('',#28717,10.);
#7984=VECTOR('',#28718,10.);
#7985=VECTOR('',#28721,10.);
#7986=VECTOR('',#28722,10.);
#7987=VECTOR('',#28725,10.);
#7988=VECTOR('',#28726,10.);
#7989=VECTOR('',#28727,10.);
#7990=VECTOR('',#28728,10.);
#7991=VECTOR('',#28729,10.);
#7992=VECTOR('',#28732,10.);
#7993=VECTOR('',#28733,10.);
#7994=VECTOR('',#28734,10.);
#7995=VECTOR('',#28735,10.);
#7996=VECTOR('',#28738,10.);
#7997=VECTOR('',#28739,10.);
#7998=VECTOR('',#28742,10.);
#7999=VECTOR('',#28743,10.);
#8000=VECTOR('',#28744,10.);
#8001=VECTOR('',#28745,10.);
#8002=VECTOR('',#28746,10.);
#8003=VECTOR('',#28749,10.);
#8004=VECTOR('',#28750,10.);
#8005=VECTOR('',#28751,10.);
#8006=VECTOR('',#28752,10.);
#8007=VECTOR('',#28755,10.);
#8008=VECTOR('',#28756,10.);
#8009=VECTOR('',#28759,10.);
#8010=VECTOR('',#28760,10.);
#8011=VECTOR('',#28761,10.);
#8012=VECTOR('',#28762,10.);
#8013=VECTOR('',#28763,10.);
#8014=VECTOR('',#28766,10.);
#8015=VECTOR('',#28767,10.);
#8016=VECTOR('',#28768,10.);
#8017=VECTOR('',#28769,10.);
#8018=VECTOR('',#28772,10.);
#8019=VECTOR('',#28773,10.);
#8020=VECTOR('',#28776,10.);
#8021=VECTOR('',#28777,10.);
#8022=VECTOR('',#28778,10.);
#8023=VECTOR('',#28779,10.);
#8024=VECTOR('',#28780,10.);
#8025=VECTOR('',#28783,10.);
#8026=VECTOR('',#28784,10.);
#8027=VECTOR('',#28785,10.);
#8028=VECTOR('',#28786,10.);
#8029=VECTOR('',#28789,10.);
#8030=VECTOR('',#28790,10.);
#8031=VECTOR('',#28793,10.);
#8032=VECTOR('',#28794,10.);
#8033=VECTOR('',#28795,10.);
#8034=VECTOR('',#28796,10.);
#8035=VECTOR('',#28797,10.);
#8036=VECTOR('',#28800,10.);
#8037=VECTOR('',#28801,10.);
#8038=VECTOR('',#28802,10.);
#8039=VECTOR('',#28803,10.);
#8040=VECTOR('',#28806,10.);
#8041=VECTOR('',#28807,10.);
#8042=VECTOR('',#28810,10.);
#8043=VECTOR('',#28811,10.);
#8044=VECTOR('',#28812,10.);
#8045=VECTOR('',#28813,10.);
#8046=VECTOR('',#28814,10.);
#8047=VECTOR('',#28817,10.);
#8048=VECTOR('',#28818,10.);
#8049=VECTOR('',#28819,10.);
#8050=VECTOR('',#28820,10.);
#8051=VECTOR('',#28823,10.);
#8052=VECTOR('',#28824,10.);
#8053=VECTOR('',#28827,10.);
#8054=VECTOR('',#28828,10.);
#8055=VECTOR('',#28829,10.);
#8056=VECTOR('',#28830,10.);
#8057=VECTOR('',#28831,10.);
#8058=VECTOR('',#28834,10.);
#8059=VECTOR('',#28835,10.);
#8060=VECTOR('',#28836,10.);
#8061=VECTOR('',#28837,10.);
#8062=VECTOR('',#28840,10.);
#8063=VECTOR('',#28841,10.);
#8064=VECTOR('',#28844,10.);
#8065=VECTOR('',#28845,10.);
#8066=VECTOR('',#28846,10.);
#8067=VECTOR('',#28847,10.);
#8068=VECTOR('',#28848,10.);
#8069=VECTOR('',#28851,10.);
#8070=VECTOR('',#28852,10.);
#8071=VECTOR('',#28853,10.);
#8072=VECTOR('',#28854,10.);
#8073=VECTOR('',#28857,10.);
#8074=VECTOR('',#28858,10.);
#8075=VECTOR('',#28861,10.);
#8076=VECTOR('',#28862,10.);
#8077=VECTOR('',#28863,10.);
#8078=VECTOR('',#28864,10.);
#8079=VECTOR('',#28865,10.);
#8080=VECTOR('',#28868,10.);
#8081=VECTOR('',#28869,10.);
#8082=VECTOR('',#28870,10.);
#8083=VECTOR('',#28871,10.);
#8084=VECTOR('',#28874,10.);
#8085=VECTOR('',#28875,10.);
#8086=VECTOR('',#28878,10.);
#8087=VECTOR('',#28879,10.);
#8088=VECTOR('',#28880,10.);
#8089=VECTOR('',#28881,10.);
#8090=VECTOR('',#28882,10.);
#8091=VECTOR('',#28885,10.);
#8092=VECTOR('',#28886,10.);
#8093=VECTOR('',#28887,10.);
#8094=VECTOR('',#28888,10.);
#8095=VECTOR('',#28891,10.);
#8096=VECTOR('',#28892,10.);
#8097=VECTOR('',#28895,10.);
#8098=VECTOR('',#28896,10.);
#8099=VECTOR('',#28897,10.);
#8100=VECTOR('',#28898,10.);
#8101=VECTOR('',#28899,10.);
#8102=VECTOR('',#28902,10.);
#8103=VECTOR('',#28903,10.);
#8104=VECTOR('',#28904,10.);
#8105=VECTOR('',#28905,10.);
#8106=VECTOR('',#28908,10.);
#8107=VECTOR('',#28909,10.);
#8108=VECTOR('',#28912,10.);
#8109=VECTOR('',#28913,10.);
#8110=VECTOR('',#28914,10.);
#8111=VECTOR('',#28915,10.);
#8112=VECTOR('',#28916,10.);
#8113=VECTOR('',#28919,10.);
#8114=VECTOR('',#28920,10.);
#8115=VECTOR('',#28921,10.);
#8116=VECTOR('',#28924,10.);
#8117=VECTOR('',#28925,10.);
#8118=VECTOR('',#28928,10.);
#8119=VECTOR('',#28929,10.);
#8120=VECTOR('',#28930,10.);
#8121=VECTOR('',#28931,10.);
#8122=VECTOR('',#28932,10.);
#8123=VECTOR('',#28935,10.);
#8124=VECTOR('',#28936,10.);
#8125=VECTOR('',#28937,10.);
#8126=VECTOR('',#28940,10.);
#8127=VECTOR('',#28941,10.);
#8128=VECTOR('',#28944,10.);
#8129=VECTOR('',#28945,10.);
#8130=VECTOR('',#28946,10.);
#8131=VECTOR('',#28947,10.);
#8132=VECTOR('',#28948,10.);
#8133=VECTOR('',#28951,10.);
#8134=VECTOR('',#28952,10.);
#8135=VECTOR('',#28953,10.);
#8136=VECTOR('',#28956,10.);
#8137=VECTOR('',#28957,10.);
#8138=VECTOR('',#28960,10.);
#8139=VECTOR('',#28961,10.);
#8140=VECTOR('',#28962,10.);
#8141=VECTOR('',#28963,10.);
#8142=VECTOR('',#28964,10.);
#8143=VECTOR('',#28967,10.);
#8144=VECTOR('',#28968,10.);
#8145=VECTOR('',#28969,10.);
#8146=VECTOR('',#28972,10.);
#8147=VECTOR('',#28973,10.);
#8148=VECTOR('',#28976,10.);
#8149=VECTOR('',#28977,10.);
#8150=VECTOR('',#28978,10.);
#8151=VECTOR('',#28979,10.);
#8152=VECTOR('',#28980,10.);
#8153=VECTOR('',#28983,10.);
#8154=VECTOR('',#28984,10.);
#8155=VECTOR('',#28985,10.);
#8156=VECTOR('',#28988,10.);
#8157=VECTOR('',#28989,10.);
#8158=VECTOR('',#28992,10.);
#8159=VECTOR('',#28993,10.);
#8160=VECTOR('',#28994,10.);
#8161=VECTOR('',#28995,10.);
#8162=VECTOR('',#28996,10.);
#8163=VECTOR('',#28999,10.);
#8164=VECTOR('',#29000,10.);
#8165=VECTOR('',#29001,10.);
#8166=VECTOR('',#29004,10.);
#8167=VECTOR('',#29005,10.);
#8168=VECTOR('',#29008,10.);
#8169=VECTOR('',#29009,10.);
#8170=VECTOR('',#29010,10.);
#8171=VECTOR('',#29011,10.);
#8172=VECTOR('',#29012,10.);
#8173=VECTOR('',#29015,10.);
#8174=VECTOR('',#29016,10.);
#8175=VECTOR('',#29017,10.);
#8176=VECTOR('',#29020,10.);
#8177=VECTOR('',#29021,10.);
#8178=VECTOR('',#29024,10.);
#8179=VECTOR('',#29025,10.);
#8180=VECTOR('',#29026,10.);
#8181=VECTOR('',#29027,10.);
#8182=VECTOR('',#29028,10.);
#8183=VECTOR('',#29031,10.);
#8184=VECTOR('',#29032,10.);
#8185=VECTOR('',#29033,10.);
#8186=VECTOR('',#29036,10.);
#8187=VECTOR('',#29037,10.);
#8188=VECTOR('',#29040,10.);
#8189=VECTOR('',#29041,10.);
#8190=VECTOR('',#29042,10.);
#8191=VECTOR('',#29043,10.);
#8192=VECTOR('',#29044,10.);
#8193=VECTOR('',#29047,10.);
#8194=VECTOR('',#29048,10.);
#8195=VECTOR('',#29049,10.);
#8196=VECTOR('',#29052,10.);
#8197=VECTOR('',#29053,10.);
#8198=VECTOR('',#29056,10.);
#8199=VECTOR('',#29057,10.);
#8200=VECTOR('',#29058,10.);
#8201=VECTOR('',#29059,10.);
#8202=VECTOR('',#29060,10.);
#8203=VECTOR('',#29063,10.);
#8204=VECTOR('',#29064,10.);
#8205=VECTOR('',#29065,10.);
#8206=VECTOR('',#29068,10.);
#8207=VECTOR('',#29069,10.);
#8208=VECTOR('',#29072,10.);
#8209=VECTOR('',#29073,10.);
#8210=VECTOR('',#29074,10.);
#8211=VECTOR('',#29075,10.);
#8212=VECTOR('',#29076,10.);
#8213=VECTOR('',#29079,10.);
#8214=VECTOR('',#29080,10.);
#8215=VECTOR('',#29081,10.);
#8216=VECTOR('',#29084,10.);
#8217=VECTOR('',#29085,10.);
#8218=VECTOR('',#29088,10.);
#8219=VECTOR('',#29089,10.);
#8220=VECTOR('',#29090,10.);
#8221=VECTOR('',#29091,10.);
#8222=VECTOR('',#29092,10.);
#8223=VECTOR('',#29095,10.);
#8224=VECTOR('',#29096,10.);
#8225=VECTOR('',#29097,10.);
#8226=VECTOR('',#29100,10.);
#8227=VECTOR('',#29101,10.);
#8228=VECTOR('',#29104,10.);
#8229=VECTOR('',#29105,10.);
#8230=VECTOR('',#29106,10.);
#8231=VECTOR('',#29107,10.);
#8232=VECTOR('',#29110,10.);
#8233=VECTOR('',#29111,10.);
#8234=VECTOR('',#29112,10.);
#8235=VECTOR('',#29113,10.);
#8236=VECTOR('',#29114,10.);
#8237=VECTOR('',#29115,10.);
#8238=VECTOR('',#29116,10.);
#8239=VECTOR('',#29117,10.);
#8240=VECTOR('',#29118,10.);
#8241=VECTOR('',#29119,10.);
#8242=VECTOR('',#29120,10.);
#8243=VECTOR('',#29121,10.);
#8244=VECTOR('',#29122,10.);
#8245=VECTOR('',#29123,10.);
#8246=VECTOR('',#29124,10.);
#8247=VECTOR('',#29125,10.);
#8248=VECTOR('',#29126,10.);
#8249=VECTOR('',#29127,10.);
#8250=VECTOR('',#29128,10.);
#8251=VECTOR('',#29129,10.);
#8252=VECTOR('',#29130,10.);
#8253=VECTOR('',#29131,10.);
#8254=VECTOR('',#29132,10.);
#8255=VECTOR('',#29133,10.);
#8256=VECTOR('',#29134,10.);
#8257=VECTOR('',#29135,10.);
#8258=VECTOR('',#29136,10.);
#8259=VECTOR('',#29137,10.);
#8260=VECTOR('',#29138,10.);
#8261=VECTOR('',#29139,10.);
#8262=VECTOR('',#29140,10.);
#8263=VECTOR('',#29141,10.);
#8264=VECTOR('',#29142,10.);
#8265=VECTOR('',#29143,10.);
#8266=VECTOR('',#29144,10.);
#8267=VECTOR('',#29145,10.);
#8268=VECTOR('',#29146,10.);
#8269=VECTOR('',#29147,10.);
#8270=VECTOR('',#29148,10.);
#8271=VECTOR('',#29149,10.);
#8272=VECTOR('',#29150,10.);
#8273=VECTOR('',#29151,10.);
#8274=VECTOR('',#29152,10.);
#8275=VECTOR('',#29153,10.);
#8276=VECTOR('',#29154,10.);
#8277=VECTOR('',#29155,10.);
#8278=VECTOR('',#29156,10.);
#8279=VECTOR('',#29157,10.);
#8280=VECTOR('',#29158,10.);
#8281=VECTOR('',#29159,10.);
#8282=VECTOR('',#29160,10.);
#8283=VECTOR('',#29161,10.);
#8284=VECTOR('',#29162,10.);
#8285=VECTOR('',#29163,10.);
#8286=VECTOR('',#29164,10.);
#8287=VECTOR('',#29165,10.);
#8288=VECTOR('',#29166,10.);
#8289=VECTOR('',#29167,10.);
#8290=VECTOR('',#29168,10.);
#8291=VECTOR('',#29169,10.);
#8292=VECTOR('',#29170,10.);
#8293=VECTOR('',#29171,10.);
#8294=VECTOR('',#29172,10.);
#8295=VECTOR('',#29173,10.);
#8296=VECTOR('',#29174,10.);
#8297=VECTOR('',#29175,10.);
#8298=VECTOR('',#29176,10.);
#8299=VECTOR('',#29177,10.);
#8300=VECTOR('',#29178,10.);
#8301=VECTOR('',#29179,10.);
#8302=VECTOR('',#29180,10.);
#8303=VECTOR('',#29181,10.);
#8304=VECTOR('',#29182,10.);
#8305=VECTOR('',#29183,10.);
#8306=VECTOR('',#29184,10.);
#8307=VECTOR('',#29185,10.);
#8308=VECTOR('',#29186,10.);
#8309=VECTOR('',#29187,10.);
#8310=VECTOR('',#29188,10.);
#8311=VECTOR('',#29189,10.);
#8312=VECTOR('',#29190,10.);
#8313=VECTOR('',#29191,10.);
#8314=VECTOR('',#29192,10.);
#8315=VECTOR('',#29193,10.);
#8316=VECTOR('',#29194,10.);
#8317=VECTOR('',#29195,10.);
#8318=VECTOR('',#29196,10.);
#8319=VECTOR('',#29197,10.);
#8320=VECTOR('',#29198,10.);
#8321=VECTOR('',#29199,10.);
#8322=VECTOR('',#29200,10.);
#8323=VECTOR('',#29201,10.);
#8324=VECTOR('',#29202,10.);
#8325=VECTOR('',#29203,10.);
#8326=VECTOR('',#29204,10.);
#8327=VECTOR('',#29205,10.);
#8328=VECTOR('',#29206,10.);
#8329=VECTOR('',#29207,10.);
#8330=VECTOR('',#29208,10.);
#8331=VECTOR('',#29209,10.);
#8332=VECTOR('',#29210,10.);
#8333=VECTOR('',#29211,10.);
#8334=VECTOR('',#29212,10.);
#8335=VECTOR('',#29213,10.);
#8336=VECTOR('',#29214,10.);
#8337=VECTOR('',#29215,10.);
#8338=VECTOR('',#29216,10.);
#8339=VECTOR('',#29217,10.);
#8340=VECTOR('',#29218,10.);
#8341=VECTOR('',#29219,10.);
#8342=VECTOR('',#29220,10.);
#8343=VECTOR('',#29221,10.);
#8344=VECTOR('',#29222,10.);
#8345=VECTOR('',#29223,10.);
#8346=VECTOR('',#29224,10.);
#8347=VECTOR('',#29225,10.);
#8348=VECTOR('',#29226,10.);
#8349=VECTOR('',#29227,10.);
#8350=VECTOR('',#29228,10.);
#8351=VECTOR('',#29229,10.);
#8352=VECTOR('',#29230,10.);
#8353=VECTOR('',#29231,10.);
#8354=VECTOR('',#29232,10.);
#8355=VECTOR('',#29233,10.);
#8356=VECTOR('',#29234,10.);
#8357=VECTOR('',#29235,10.);
#8358=VECTOR('',#29236,10.);
#8359=VECTOR('',#29237,10.);
#8360=VECTOR('',#29238,10.);
#8361=VECTOR('',#29239,10.);
#8362=VECTOR('',#29240,10.);
#8363=VECTOR('',#29241,10.);
#8364=VECTOR('',#29242,10.);
#8365=VECTOR('',#29243,10.);
#8366=VECTOR('',#29244,10.);
#8367=VECTOR('',#29245,10.);
#8368=VECTOR('',#29246,10.);
#8369=VECTOR('',#29247,10.);
#8370=VECTOR('',#29248,10.);
#8371=VECTOR('',#29249,10.);
#8372=VECTOR('',#29250,10.);
#8373=VECTOR('',#29251,10.);
#8374=VECTOR('',#29252,10.);
#8375=VECTOR('',#29253,10.);
#8376=VECTOR('',#29254,10.);
#8377=VECTOR('',#29255,10.);
#8378=VECTOR('',#29256,10.);
#8379=VECTOR('',#29257,10.);
#8380=VECTOR('',#29258,10.);
#8381=VECTOR('',#29259,10.);
#8382=VECTOR('',#29260,10.);
#8383=VECTOR('',#29261,10.);
#8384=VECTOR('',#29262,10.);
#8385=VECTOR('',#29263,10.);
#8386=VECTOR('',#29264,10.);
#8387=VECTOR('',#29265,10.);
#8388=VECTOR('',#29266,10.);
#8389=VECTOR('',#29267,10.);
#8390=VECTOR('',#29268,10.);
#8391=VECTOR('',#29269,10.);
#8392=VECTOR('',#29270,10.);
#8393=VECTOR('',#29271,10.);
#8394=VECTOR('',#29272,10.);
#8395=VECTOR('',#29273,10.);
#8396=VECTOR('',#29274,10.);
#8397=VECTOR('',#29275,10.);
#8398=VECTOR('',#29276,10.);
#8399=VECTOR('',#29277,10.);
#8400=VECTOR('',#29278,10.);
#8401=VECTOR('',#29279,10.);
#8402=VECTOR('',#29280,10.);
#8403=VECTOR('',#29281,10.);
#8404=VECTOR('',#29282,10.);
#8405=VECTOR('',#29283,10.);
#8406=VECTOR('',#29284,10.);
#8407=VECTOR('',#29285,10.);
#8408=VECTOR('',#29286,10.);
#8409=VECTOR('',#29287,10.);
#8410=VECTOR('',#29288,10.);
#8411=VECTOR('',#29289,10.);
#8412=VECTOR('',#29290,10.);
#8413=VECTOR('',#29291,10.);
#8414=VECTOR('',#29292,10.);
#8415=VECTOR('',#29293,10.);
#8416=VECTOR('',#29294,10.);
#8417=VECTOR('',#29295,10.);
#8418=VECTOR('',#29296,10.);
#8419=VECTOR('',#29297,10.);
#8420=VECTOR('',#29298,10.);
#8421=VECTOR('',#29299,10.);
#8422=VECTOR('',#29300,10.);
#8423=VECTOR('',#29301,10.);
#8424=VECTOR('',#29302,10.);
#8425=VECTOR('',#29303,10.);
#8426=VECTOR('',#29304,10.);
#8427=VECTOR('',#29305,10.);
#8428=VECTOR('',#29306,10.);
#8429=VECTOR('',#29307,10.);
#8430=VECTOR('',#29308,10.);
#8431=VECTOR('',#29309,10.);
#8432=VECTOR('',#29310,10.);
#8433=VECTOR('',#29311,10.);
#8434=VECTOR('',#29312,10.);
#8435=VECTOR('',#29313,10.);
#8436=VECTOR('',#29314,10.);
#8437=VECTOR('',#29315,10.);
#8438=VECTOR('',#29316,10.);
#8439=VECTOR('',#29317,10.);
#8440=VECTOR('',#29318,10.);
#8441=VECTOR('',#29319,10.);
#8442=VECTOR('',#29320,10.);
#8443=VECTOR('',#29321,10.);
#8444=VECTOR('',#29322,10.);
#8445=VECTOR('',#29323,10.);
#8446=VECTOR('',#29324,10.);
#8447=VECTOR('',#29325,10.);
#8448=VECTOR('',#29326,10.);
#8449=VECTOR('',#29327,10.);
#8450=VECTOR('',#29328,10.);
#8451=VECTOR('',#29329,10.);
#8452=VECTOR('',#29330,10.);
#8453=VECTOR('',#29331,10.);
#8454=VECTOR('',#29332,10.);
#8455=VECTOR('',#29333,10.);
#8456=VECTOR('',#29334,10.);
#8457=VECTOR('',#29335,10.);
#8458=VECTOR('',#29336,10.);
#8459=VECTOR('',#29341,10.);
#8460=VECTOR('',#29342,10.);
#8461=VECTOR('',#29343,10.);
#8462=VECTOR('',#29346,10.);
#8463=VECTOR('',#29347,10.);
#8464=VECTOR('',#29348,10.);
#8465=VECTOR('',#29351,10.);
#8466=VECTOR('',#29352,10.);
#8467=VECTOR('',#29353,10.);
#8468=VECTOR('',#29356,10.);
#8469=VECTOR('',#29357,10.);
#8470=VECTOR('',#29358,10.);
#8471=VECTOR('',#29361,10.);
#8472=VECTOR('',#29362,10.);
#8473=VECTOR('',#29363,10.);
#8474=VECTOR('',#29366,10.);
#8475=VECTOR('',#29367,10.);
#8476=VECTOR('',#29368,10.);
#8477=VECTOR('',#29371,10.);
#8478=VECTOR('',#29372,10.);
#8479=VECTOR('',#29373,10.);
#8480=VECTOR('',#29376,10.);
#8481=VECTOR('',#29377,10.);
#8482=VECTOR('',#29378,10.);
#8483=VECTOR('',#29381,10.);
#8484=VECTOR('',#29382,10.);
#8485=VECTOR('',#29383,10.);
#8486=VECTOR('',#29386,10.);
#8487=VECTOR('',#29387,10.);
#8488=VECTOR('',#29388,10.);
#8489=VECTOR('',#29391,10.);
#8490=VECTOR('',#29392,10.);
#8491=VECTOR('',#29393,10.);
#8492=VECTOR('',#29396,10.);
#8493=VECTOR('',#29397,10.);
#8494=VECTOR('',#29398,10.);
#8495=VECTOR('',#29401,10.);
#8496=VECTOR('',#29402,10.);
#8497=VECTOR('',#29403,10.);
#8498=VECTOR('',#29406,10.);
#8499=VECTOR('',#29407,10.);
#8500=VECTOR('',#29408,10.);
#8501=VECTOR('',#29411,10.);
#8502=VECTOR('',#29412,10.);
#8503=VECTOR('',#29413,10.);
#8504=VECTOR('',#29416,10.);
#8505=VECTOR('',#29417,10.);
#8506=VECTOR('',#29418,10.);
#8507=VECTOR('',#29421,10.);
#8508=VECTOR('',#29422,10.);
#8509=VECTOR('',#29423,10.);
#8510=VECTOR('',#29426,10.);
#8511=VECTOR('',#29427,10.);
#8512=VECTOR('',#29428,10.);
#8513=VECTOR('',#29431,10.);
#8514=VECTOR('',#29432,10.);
#8515=VECTOR('',#29433,10.);
#8516=VECTOR('',#29436,10.);
#8517=VECTOR('',#29437,10.);
#8518=VECTOR('',#29438,10.);
#8519=VECTOR('',#29441,10.);
#8520=VECTOR('',#29442,10.);
#8521=VECTOR('',#29443,10.);
#8522=VECTOR('',#29446,10.);
#8523=VECTOR('',#29447,10.);
#8524=VECTOR('',#29448,10.);
#8525=VECTOR('',#29451,10.);
#8526=VECTOR('',#29452,10.);
#8527=VECTOR('',#29453,10.);
#8528=VECTOR('',#29458,10.);
#8529=VECTOR('',#29459,10.);
#8530=VECTOR('',#29460,10.);
#8531=VECTOR('',#29463,10.);
#8532=VECTOR('',#29464,10.);
#8533=VECTOR('',#29465,10.);
#8534=VECTOR('',#29468,10.);
#8535=VECTOR('',#29469,10.);
#8536=VECTOR('',#29470,10.);
#8537=VECTOR('',#29475,10.);
#8538=VECTOR('',#29480,10.);
#8539=VECTOR('',#29481,10.);
#8540=VECTOR('',#29484,10.);
#8541=VECTOR('',#29489,10.);
#8542=VECTOR('',#29492,10.);
#8543=VECTOR('',#29495,10.);
#8544=VECTOR('',#29498,10.);
#8545=VECTOR('',#29501,10.);
#8546=VECTOR('',#29504,10.);
#8547=VECTOR('',#29507,10.);
#8548=VECTOR('',#29510,10.);
#8549=VECTOR('',#29513,10.);
#8550=VECTOR('',#29516,10.);
#8551=VECTOR('',#29519,10.);
#8552=VECTOR('',#29522,10.);
#8553=VECTOR('',#29525,10.);
#8554=VECTOR('',#29528,10.);
#8555=VECTOR('',#29531,10.);
#8556=VECTOR('',#29536,10.);
#8557=VECTOR('',#29539,10.);
#8558=VECTOR('',#29542,10.);
#8559=VECTOR('',#29547,10.);
#8560=VECTOR('',#29550,10.);
#8561=VECTOR('',#29553,10.);
#8562=VECTOR('',#29556,10.);
#8563=VECTOR('',#29559,10.);
#8564=VECTOR('',#29562,10.);
#8565=VECTOR('',#29565,10.);
#8566=VECTOR('',#29568,10.);
#8567=VECTOR('',#29571,10.);
#8568=VECTOR('',#29574,10.);
#8569=VECTOR('',#29577,10.);
#8570=VECTOR('',#29580,10.);
#8571=VECTOR('',#29583,10.);
#8572=VECTOR('',#29586,10.);
#8573=VECTOR('',#29589,10.);
#8574=VECTOR('',#29594,10.);
#8575=VECTOR('',#29597,10.);
#8576=VECTOR('',#29600,10.);
#8577=VECTOR('',#29605,10.);
#8578=VECTOR('',#29608,10.);
#8579=VECTOR('',#29611,10.);
#8580=VECTOR('',#29614,10.);
#8581=VECTOR('',#29617,10.);
#8582=VECTOR('',#29620,10.);
#8583=VECTOR('',#29623,10.);
#8584=VECTOR('',#29626,10.);
#8585=VECTOR('',#29629,10.);
#8586=VECTOR('',#29632,10.);
#8587=VECTOR('',#29635,10.);
#8588=VECTOR('',#29638,10.);
#8589=VECTOR('',#29641,10.);
#8590=VECTOR('',#29644,10.);
#8591=VECTOR('',#29647,10.);
#8592=VECTOR('',#29652,10.);
#8593=VECTOR('',#29655,10.);
#8594=VECTOR('',#29658,10.);
#8595=VECTOR('',#29663,10.);
#8596=VECTOR('',#29666,10.);
#8597=VECTOR('',#29669,10.);
#8598=VECTOR('',#29672,10.);
#8599=VECTOR('',#29675,10.);
#8600=VECTOR('',#29678,10.);
#8601=VECTOR('',#29681,10.);
#8602=VECTOR('',#29684,10.);
#8603=VECTOR('',#29687,10.);
#8604=VECTOR('',#29690,10.);
#8605=VECTOR('',#29693,10.);
#8606=VECTOR('',#29696,10.);
#8607=VECTOR('',#29699,10.);
#8608=VECTOR('',#29702,10.);
#8609=VECTOR('',#29705,10.);
#8610=VECTOR('',#29710,10.);
#8611=VECTOR('',#29713,10.);
#8612=VECTOR('',#29716,10.);
#8613=VECTOR('',#29721,10.);
#8614=VECTOR('',#29724,10.);
#8615=VECTOR('',#29727,10.);
#8616=VECTOR('',#29730,10.);
#8617=VECTOR('',#29733,10.);
#8618=VECTOR('',#29736,10.);
#8619=VECTOR('',#29739,10.);
#8620=VECTOR('',#29742,10.);
#8621=VECTOR('',#29745,10.);
#8622=VECTOR('',#29748,10.);
#8623=VECTOR('',#29751,10.);
#8624=VECTOR('',#29754,10.);
#8625=VECTOR('',#29757,10.);
#8626=VECTOR('',#29760,10.);
#8627=VECTOR('',#29763,10.);
#8628=VECTOR('',#29768,10.);
#8629=VECTOR('',#29771,10.);
#8630=VECTOR('',#29774,10.);
#8631=VECTOR('',#29779,10.);
#8632=VECTOR('',#29782,10.);
#8633=VECTOR('',#29785,10.);
#8634=VECTOR('',#29788,10.);
#8635=VECTOR('',#29791,10.);
#8636=VECTOR('',#29794,10.);
#8637=VECTOR('',#29797,10.);
#8638=VECTOR('',#29800,10.);
#8639=VECTOR('',#29803,10.);
#8640=VECTOR('',#29806,10.);
#8641=VECTOR('',#29809,10.);
#8642=VECTOR('',#29812,10.);
#8643=VECTOR('',#29815,10.);
#8644=VECTOR('',#29818,10.);
#8645=VECTOR('',#29821,10.);
#8646=VECTOR('',#29826,10.);
#8647=VECTOR('',#29829,10.);
#8648=VECTOR('',#29832,10.);
#8649=VECTOR('',#29837,10.);
#8650=VECTOR('',#29840,10.);
#8651=VECTOR('',#29843,10.);
#8652=VECTOR('',#29846,10.);
#8653=VECTOR('',#29849,10.);
#8654=VECTOR('',#29852,10.);
#8655=VECTOR('',#29855,10.);
#8656=VECTOR('',#29858,10.);
#8657=VECTOR('',#29861,10.);
#8658=VECTOR('',#29864,10.);
#8659=VECTOR('',#29867,10.);
#8660=VECTOR('',#29870,10.);
#8661=VECTOR('',#29873,10.);
#8662=VECTOR('',#29876,10.);
#8663=VECTOR('',#29879,10.);
#8664=VECTOR('',#29884,10.);
#8665=VECTOR('',#29887,10.);
#8666=VECTOR('',#29890,10.);
#8667=VECTOR('',#29895,10.);
#8668=VECTOR('',#29898,10.);
#8669=VECTOR('',#29901,10.);
#8670=VECTOR('',#29904,10.);
#8671=VECTOR('',#29907,10.);
#8672=VECTOR('',#29910,10.);
#8673=VECTOR('',#29913,10.);
#8674=VECTOR('',#29916,10.);
#8675=VECTOR('',#29919,10.);
#8676=VECTOR('',#29922,10.);
#8677=VECTOR('',#29925,10.);
#8678=VECTOR('',#29928,10.);
#8679=VECTOR('',#29931,10.);
#8680=VECTOR('',#29934,10.);
#8681=VECTOR('',#29937,10.);
#8682=VECTOR('',#29942,10.);
#8683=VECTOR('',#29945,10.);
#8684=VECTOR('',#29948,10.);
#8685=VECTOR('',#29953,10.);
#8686=VECTOR('',#29956,10.);
#8687=VECTOR('',#29959,10.);
#8688=VECTOR('',#29962,10.);
#8689=VECTOR('',#29965,10.);
#8690=VECTOR('',#29968,10.);
#8691=VECTOR('',#29971,10.);
#8692=VECTOR('',#29974,10.);
#8693=VECTOR('',#29977,10.);
#8694=VECTOR('',#29980,10.);
#8695=VECTOR('',#29983,10.);
#8696=VECTOR('',#29986,10.);
#8697=VECTOR('',#29989,10.);
#8698=VECTOR('',#29992,10.);
#8699=VECTOR('',#29995,10.);
#8700=VECTOR('',#30000,10.);
#8701=VECTOR('',#30003,10.);
#8702=VECTOR('',#30006,10.);
#8703=VECTOR('',#30011,10.);
#8704=VECTOR('',#30014,10.);
#8705=VECTOR('',#30017,10.);
#8706=VECTOR('',#30020,10.);
#8707=VECTOR('',#30023,10.);
#8708=VECTOR('',#30026,10.);
#8709=VECTOR('',#30029,10.);
#8710=VECTOR('',#30032,10.);
#8711=VECTOR('',#30035,10.);
#8712=VECTOR('',#30038,10.);
#8713=VECTOR('',#30041,10.);
#8714=VECTOR('',#30044,10.);
#8715=VECTOR('',#30047,10.);
#8716=VECTOR('',#30050,10.);
#8717=VECTOR('',#30053,10.);
#8718=VECTOR('',#30058,10.);
#8719=VECTOR('',#30061,10.);
#8720=VECTOR('',#30064,10.);
#8721=VECTOR('',#30069,10.);
#8722=VECTOR('',#30072,10.);
#8723=VECTOR('',#30075,10.);
#8724=VECTOR('',#30078,10.);
#8725=VECTOR('',#30081,10.);
#8726=VECTOR('',#30084,10.);
#8727=VECTOR('',#30087,10.);
#8728=VECTOR('',#30090,10.);
#8729=VECTOR('',#30093,10.);
#8730=VECTOR('',#30096,10.);
#8731=VECTOR('',#30099,10.);
#8732=VECTOR('',#30102,10.);
#8733=VECTOR('',#30105,10.);
#8734=VECTOR('',#30108,10.);
#8735=VECTOR('',#30111,10.);
#8736=VECTOR('',#30116,10.);
#8737=VECTOR('',#30119,10.);
#8738=VECTOR('',#30122,10.);
#8739=VECTOR('',#30127,10.);
#8740=VECTOR('',#30130,10.);
#8741=VECTOR('',#30133,10.);
#8742=VECTOR('',#30136,10.);
#8743=VECTOR('',#30139,10.);
#8744=VECTOR('',#30142,10.);
#8745=VECTOR('',#30145,10.);
#8746=VECTOR('',#30148,10.);
#8747=VECTOR('',#30151,10.);
#8748=VECTOR('',#30154,10.);
#8749=VECTOR('',#30157,10.);
#8750=VECTOR('',#30160,10.);
#8751=VECTOR('',#30163,10.);
#8752=VECTOR('',#30166,10.);
#8753=VECTOR('',#30169,10.);
#8754=VECTOR('',#30176,8.5);
#8755=VECTOR('',#30187,7.69);
#8756=VECTOR('',#30192,7.94);
#8757=VECTOR('',#30199,8.5);
#8758=VECTOR('',#30206,10.);
#8759=VECTOR('',#30207,10.);
#8760=VECTOR('',#30208,10.);
#8761=VECTOR('',#30209,10.);
#8762=VECTOR('',#30210,10.);
#8763=VECTOR('',#30211,10.);
#8764=VECTOR('',#30214,10.);
#8765=VECTOR('',#30215,10.);
#8766=VECTOR('',#30216,10.);
#8767=VECTOR('',#30217,10.);
#8768=VECTOR('',#30218,10.);
#8769=VECTOR('',#30219,10.);
#8770=VECTOR('',#30220,10.);
#8771=VECTOR('',#30221,10.);
#8772=VECTOR('',#30222,10.);
#8773=VECTOR('',#30223,10.);
#8774=VECTOR('',#30224,10.);
#8775=VECTOR('',#30225,10.);
#8776=VECTOR('',#30226,10.);
#8777=VECTOR('',#30227,10.);
#8778=VECTOR('',#30228,10.);
#8779=VECTOR('',#30229,10.);
#8780=VECTOR('',#30230,10.);
#8781=VECTOR('',#30231,10.);
#8782=VECTOR('',#30232,10.);
#8783=VECTOR('',#30233,10.);
#8784=VECTOR('',#30234,10.);
#8785=VECTOR('',#30235,10.);
#8786=VECTOR('',#30236,10.);
#8787=VECTOR('',#30237,10.);
#8788=VECTOR('',#30238,10.);
#8789=VECTOR('',#30239,10.);
#8790=VECTOR('',#30240,10.);
#8791=VECTOR('',#30241,10.);
#8792=VECTOR('',#30242,10.);
#8793=VECTOR('',#30243,10.);
#8794=VECTOR('',#30244,10.);
#8795=VECTOR('',#30245,10.);
#8796=VECTOR('',#30246,10.);
#8797=VECTOR('',#30247,10.);
#8798=VECTOR('',#30248,10.);
#8799=VECTOR('',#30249,10.);
#8800=VECTOR('',#30250,10.);
#8801=VECTOR('',#30251,10.);
#8802=VECTOR('',#30252,10.);
#8803=VECTOR('',#30253,10.);
#8804=VECTOR('',#30254,10.);
#8805=VECTOR('',#30255,10.);
#8806=VECTOR('',#30256,10.);
#8807=VECTOR('',#30257,10.);
#8808=VECTOR('',#30258,10.);
#8809=VECTOR('',#30259,10.);
#8810=VECTOR('',#30260,10.);
#8811=VECTOR('',#30261,10.);
#8812=VECTOR('',#30262,10.);
#8813=VECTOR('',#30263,10.);
#8814=VECTOR('',#30264,10.);
#8815=VECTOR('',#30265,10.);
#8816=VECTOR('',#30266,10.);
#8817=VECTOR('',#30267,10.);
#8818=VECTOR('',#30268,10.);
#8819=VECTOR('',#30269,10.);
#8820=VECTOR('',#30270,10.);
#8821=VECTOR('',#30271,10.);
#8822=VECTOR('',#30272,10.);
#8823=VECTOR('',#30273,10.);
#8824=VECTOR('',#30274,10.);
#8825=VECTOR('',#30275,10.);
#8826=VECTOR('',#30276,10.);
#8827=VECTOR('',#30277,10.);
#8828=VECTOR('',#30278,10.);
#8829=VECTOR('',#30279,10.);
#8830=VECTOR('',#30280,10.);
#8831=VECTOR('',#30281,10.);
#8832=VECTOR('',#30282,10.);
#8833=VECTOR('',#30283,10.);
#8834=VECTOR('',#30284,10.);
#8835=VECTOR('',#30285,10.);
#8836=VECTOR('',#30286,10.);
#8837=VECTOR('',#30287,10.);
#8838=VECTOR('',#30288,10.);
#8839=VECTOR('',#30289,10.);
#8840=VECTOR('',#30290,10.);
#8841=VECTOR('',#30291,10.);
#8842=VECTOR('',#30292,10.);
#8843=VECTOR('',#30293,10.);
#8844=VECTOR('',#30294,10.);
#8845=VECTOR('',#30295,10.);
#8846=VECTOR('',#30296,10.);
#8847=VECTOR('',#30297,10.);
#8848=VECTOR('',#30298,10.);
#8849=VECTOR('',#30299,10.);
#8850=VECTOR('',#30300,10.);
#8851=VECTOR('',#30301,10.);
#8852=VECTOR('',#30302,10.);
#8853=VECTOR('',#30303,10.);
#8854=VECTOR('',#30304,10.);
#8855=VECTOR('',#30305,10.);
#8856=VECTOR('',#30306,10.);
#8857=VECTOR('',#30307,10.);
#8858=VECTOR('',#30308,10.);
#8859=VECTOR('',#30309,10.);
#8860=VECTOR('',#30310,10.);
#8861=VECTOR('',#30311,10.);
#8862=VECTOR('',#30312,10.);
#8863=VECTOR('',#30313,10.);
#8864=VECTOR('',#30314,10.);
#8865=VECTOR('',#30315,10.);
#8866=VECTOR('',#30316,10.);
#8867=VECTOR('',#30317,10.);
#8868=VECTOR('',#30318,10.);
#8869=VECTOR('',#30319,10.);
#8870=VECTOR('',#30320,10.);
#8871=VECTOR('',#30321,10.);
#8872=VECTOR('',#30322,10.);
#8873=VECTOR('',#30323,10.);
#8874=VECTOR('',#30324,10.);
#8875=VECTOR('',#30325,10.);
#8876=VECTOR('',#30326,10.);
#8877=VECTOR('',#30327,10.);
#8878=VECTOR('',#30328,10.);
#8879=VECTOR('',#30329,10.);
#8880=VECTOR('',#30330,10.);
#8881=VECTOR('',#30331,10.);
#8882=VECTOR('',#30332,10.);
#8883=VECTOR('',#30333,10.);
#8884=VECTOR('',#30334,10.);
#8885=VECTOR('',#30335,10.);
#8886=VECTOR('',#30336,10.);
#8887=VECTOR('',#30337,10.);
#8888=VECTOR('',#30338,10.);
#8889=VECTOR('',#30339,10.);
#8890=VECTOR('',#30340,10.);
#8891=VECTOR('',#30341,10.);
#8892=VECTOR('',#30342,10.);
#8893=VECTOR('',#30343,10.);
#8894=VECTOR('',#30344,10.);
#8895=VECTOR('',#30345,10.);
#8896=VECTOR('',#30346,10.);
#8897=VECTOR('',#30347,10.);
#8898=VECTOR('',#30348,10.);
#8899=VECTOR('',#30349,10.);
#8900=VECTOR('',#30350,10.);
#8901=VECTOR('',#30351,10.);
#8902=VECTOR('',#30352,10.);
#8903=VECTOR('',#30353,10.);
#8904=VECTOR('',#30354,10.);
#8905=VECTOR('',#30355,10.);
#8906=VECTOR('',#30356,10.);
#8907=VECTOR('',#30357,10.);
#8908=VECTOR('',#30358,10.);
#8909=VECTOR('',#30359,10.);
#8910=VECTOR('',#30360,10.);
#8911=VECTOR('',#30361,10.);
#8912=VECTOR('',#30362,10.);
#8913=VECTOR('',#30363,10.);
#8914=VECTOR('',#30364,10.);
#8915=VECTOR('',#30365,10.);
#8916=VECTOR('',#30366,10.);
#8917=VECTOR('',#30367,10.);
#8918=VECTOR('',#30368,10.);
#8919=VECTOR('',#30369,10.);
#8920=VECTOR('',#30370,10.);
#8921=VECTOR('',#30371,10.);
#8922=VECTOR('',#30372,10.);
#8923=VECTOR('',#30373,10.);
#8924=VECTOR('',#30374,10.);
#8925=VECTOR('',#30375,10.);
#8926=VECTOR('',#30376,10.);
#8927=VECTOR('',#30377,10.);
#8928=VECTOR('',#30378,10.);
#8929=VECTOR('',#30379,10.);
#8930=VECTOR('',#30380,10.);
#8931=VECTOR('',#30381,10.);
#8932=VECTOR('',#30382,10.);
#8933=VECTOR('',#30383,10.);
#8934=VECTOR('',#30384,10.);
#8935=VECTOR('',#30385,10.);
#8936=VECTOR('',#30386,10.);
#8937=VECTOR('',#30387,10.);
#8938=VECTOR('',#30388,10.);
#8939=VECTOR('',#30389,10.);
#8940=VECTOR('',#30390,10.);
#8941=VECTOR('',#30391,10.);
#8942=VECTOR('',#30392,10.);
#8943=VECTOR('',#30393,10.);
#8944=VECTOR('',#30394,10.);
#8945=VECTOR('',#30395,10.);
#8946=VECTOR('',#30396,10.);
#8947=VECTOR('',#30397,10.);
#8948=VECTOR('',#30398,10.);
#8949=VECTOR('',#30399,10.);
#8950=VECTOR('',#30400,10.);
#8951=VECTOR('',#30401,10.);
#8952=VECTOR('',#30402,10.);
#8953=VECTOR('',#30403,10.);
#8954=VECTOR('',#30404,10.);
#8955=VECTOR('',#30405,10.);
#8956=VECTOR('',#30406,10.);
#8957=VECTOR('',#30407,10.);
#8958=VECTOR('',#30408,10.);
#8959=VECTOR('',#30409,10.);
#8960=VECTOR('',#30410,10.);
#8961=VECTOR('',#30411,10.);
#8962=VECTOR('',#30412,10.);
#8963=VECTOR('',#30413,10.);
#8964=VECTOR('',#30414,10.);
#8965=VECTOR('',#30415,10.);
#8966=VECTOR('',#30416,10.);
#8967=VECTOR('',#30417,10.);
#8968=VECTOR('',#30418,10.);
#8969=VECTOR('',#30419,10.);
#8970=VECTOR('',#30420,10.);
#8971=VECTOR('',#30421,10.);
#8972=VECTOR('',#30422,10.);
#8973=VECTOR('',#30423,10.);
#8974=VECTOR('',#30424,10.);
#8975=VECTOR('',#30425,10.);
#8976=VECTOR('',#30426,10.);
#8977=VECTOR('',#30427,10.);
#8978=VECTOR('',#30428,10.);
#8979=VECTOR('',#30429,10.);
#8980=VECTOR('',#30430,10.);
#8981=VECTOR('',#30431,10.);
#8982=VECTOR('',#30432,10.);
#8983=VECTOR('',#30433,10.);
#8984=VECTOR('',#30434,10.);
#8985=VECTOR('',#30435,10.);
#8986=VECTOR('',#30436,10.);
#8987=VECTOR('',#30437,10.);
#8988=VECTOR('',#30438,10.);
#8989=VECTOR('',#30439,10.);
#8990=VECTOR('',#30440,10.);
#8991=VECTOR('',#30441,10.);
#8992=VECTOR('',#30442,10.);
#8993=VECTOR('',#30443,10.);
#8994=VECTOR('',#30444,10.);
#8995=VECTOR('',#30445,10.);
#8996=VECTOR('',#30446,10.);
#8997=VECTOR('',#30447,10.);
#8998=VECTOR('',#30448,10.);
#8999=VECTOR('',#30449,10.);
#9000=VECTOR('',#30450,10.);
#9001=VECTOR('',#30451,10.);
#9002=VECTOR('',#30452,10.);
#9003=VECTOR('',#30457,10.);
#9004=VECTOR('',#30458,10.);
#9005=VECTOR('',#30459,10.);
#9006=VECTOR('',#30460,10.);
#9007=VECTOR('',#30463,10.);
#9008=VECTOR('',#30464,10.);
#9009=VECTOR('',#30467,10.);
#9010=VECTOR('',#30468,10.);
#9011=VECTOR('',#30469,10.);
#9012=VECTOR('',#30470,10.);
#9013=VECTOR('',#30471,10.);
#9014=VECTOR('',#30474,10.);
#9015=VECTOR('',#30475,10.);
#9016=VECTOR('',#30476,10.);
#9017=VECTOR('',#30477,10.);
#9018=VECTOR('',#30480,10.);
#9019=VECTOR('',#30481,10.);
#9020=VECTOR('',#30484,10.);
#9021=VECTOR('',#30485,10.);
#9022=VECTOR('',#30486,10.);
#9023=VECTOR('',#30487,10.);
#9024=VECTOR('',#30488,10.);
#9025=VECTOR('',#30491,10.);
#9026=VECTOR('',#30492,10.);
#9027=VECTOR('',#30493,10.);
#9028=VECTOR('',#30494,10.);
#9029=VECTOR('',#30497,10.);
#9030=VECTOR('',#30498,10.);
#9031=VECTOR('',#30501,10.);
#9032=VECTOR('',#30502,10.);
#9033=VECTOR('',#30503,10.);
#9034=VECTOR('',#30504,10.);
#9035=VECTOR('',#30505,10.);
#9036=VECTOR('',#30508,10.);
#9037=VECTOR('',#30509,10.);
#9038=VECTOR('',#30510,10.);
#9039=VECTOR('',#30511,10.);
#9040=VECTOR('',#30514,10.);
#9041=VECTOR('',#30515,10.);
#9042=VECTOR('',#30518,10.);
#9043=VECTOR('',#30519,10.);
#9044=VECTOR('',#30520,10.);
#9045=VECTOR('',#30521,10.);
#9046=VECTOR('',#30522,10.);
#9047=VECTOR('',#30525,10.);
#9048=VECTOR('',#30526,10.);
#9049=VECTOR('',#30527,10.);
#9050=VECTOR('',#30528,10.);
#9051=VECTOR('',#30531,10.);
#9052=VECTOR('',#30532,10.);
#9053=VECTOR('',#30535,10.);
#9054=VECTOR('',#30536,10.);
#9055=VECTOR('',#30537,10.);
#9056=VECTOR('',#30538,10.);
#9057=VECTOR('',#30539,10.);
#9058=VECTOR('',#30542,10.);
#9059=VECTOR('',#30543,10.);
#9060=VECTOR('',#30544,10.);
#9061=VECTOR('',#30545,10.);
#9062=VECTOR('',#30548,10.);
#9063=VECTOR('',#30549,10.);
#9064=VECTOR('',#30552,10.);
#9065=VECTOR('',#30553,10.);
#9066=VECTOR('',#30554,10.);
#9067=VECTOR('',#30555,10.);
#9068=VECTOR('',#30556,10.);
#9069=VECTOR('',#30559,10.);
#9070=VECTOR('',#30560,10.);
#9071=VECTOR('',#30561,10.);
#9072=VECTOR('',#30562,10.);
#9073=VECTOR('',#30565,10.);
#9074=VECTOR('',#30566,10.);
#9075=VECTOR('',#30569,10.);
#9076=VECTOR('',#30570,10.);
#9077=VECTOR('',#30571,10.);
#9078=VECTOR('',#30572,10.);
#9079=VECTOR('',#30573,10.);
#9080=VECTOR('',#30576,10.);
#9081=VECTOR('',#30577,10.);
#9082=VECTOR('',#30578,10.);
#9083=VECTOR('',#30579,10.);
#9084=VECTOR('',#30582,10.);
#9085=VECTOR('',#30583,10.);
#9086=VECTOR('',#30586,10.);
#9087=VECTOR('',#30587,10.);
#9088=VECTOR('',#30588,10.);
#9089=VECTOR('',#30589,10.);
#9090=VECTOR('',#30590,10.);
#9091=VECTOR('',#30593,10.);
#9092=VECTOR('',#30594,10.);
#9093=VECTOR('',#30595,10.);
#9094=VECTOR('',#30596,10.);
#9095=VECTOR('',#30599,10.);
#9096=VECTOR('',#30600,10.);
#9097=VECTOR('',#30603,10.);
#9098=VECTOR('',#30604,10.);
#9099=VECTOR('',#30605,10.);
#9100=VECTOR('',#30606,10.);
#9101=VECTOR('',#30607,10.);
#9102=VECTOR('',#30610,10.);
#9103=VECTOR('',#30611,10.);
#9104=VECTOR('',#30612,10.);
#9105=VECTOR('',#30613,10.);
#9106=VECTOR('',#30616,10.);
#9107=VECTOR('',#30617,10.);
#9108=VECTOR('',#30620,10.);
#9109=VECTOR('',#30621,10.);
#9110=VECTOR('',#30622,10.);
#9111=VECTOR('',#30623,10.);
#9112=VECTOR('',#30624,10.);
#9113=VECTOR('',#30627,10.);
#9114=VECTOR('',#30628,10.);
#9115=VECTOR('',#30629,10.);
#9116=VECTOR('',#30630,10.);
#9117=VECTOR('',#30633,10.);
#9118=VECTOR('',#30634,10.);
#9119=VECTOR('',#30637,10.);
#9120=VECTOR('',#30638,10.);
#9121=VECTOR('',#30639,10.);
#9122=VECTOR('',#30640,10.);
#9123=VECTOR('',#30641,10.);
#9124=VECTOR('',#30644,10.);
#9125=VECTOR('',#30645,10.);
#9126=VECTOR('',#30646,10.);
#9127=VECTOR('',#30647,10.);
#9128=VECTOR('',#30650,10.);
#9129=VECTOR('',#30651,10.);
#9130=VECTOR('',#30654,10.);
#9131=VECTOR('',#30655,10.);
#9132=VECTOR('',#30656,10.);
#9133=VECTOR('',#30657,10.);
#9134=VECTOR('',#30658,10.);
#9135=VECTOR('',#30661,10.);
#9136=VECTOR('',#30662,10.);
#9137=VECTOR('',#30663,10.);
#9138=VECTOR('',#30666,10.);
#9139=VECTOR('',#30667,10.);
#9140=VECTOR('',#30670,10.);
#9141=VECTOR('',#30671,10.);
#9142=VECTOR('',#30672,10.);
#9143=VECTOR('',#30673,10.);
#9144=VECTOR('',#30674,10.);
#9145=VECTOR('',#30677,10.);
#9146=VECTOR('',#30678,10.);
#9147=VECTOR('',#30679,10.);
#9148=VECTOR('',#30682,10.);
#9149=VECTOR('',#30683,10.);
#9150=VECTOR('',#30686,10.);
#9151=VECTOR('',#30687,10.);
#9152=VECTOR('',#30688,10.);
#9153=VECTOR('',#30689,10.);
#9154=VECTOR('',#30690,10.);
#9155=VECTOR('',#30693,10.);
#9156=VECTOR('',#30694,10.);
#9157=VECTOR('',#30695,10.);
#9158=VECTOR('',#30698,10.);
#9159=VECTOR('',#30699,10.);
#9160=VECTOR('',#30702,10.);
#9161=VECTOR('',#30703,10.);
#9162=VECTOR('',#30704,10.);
#9163=VECTOR('',#30705,10.);
#9164=VECTOR('',#30706,10.);
#9165=VECTOR('',#30709,10.);
#9166=VECTOR('',#30710,10.);
#9167=VECTOR('',#30711,10.);
#9168=VECTOR('',#30714,10.);
#9169=VECTOR('',#30715,10.);
#9170=VECTOR('',#30718,10.);
#9171=VECTOR('',#30719,10.);
#9172=VECTOR('',#30720,10.);
#9173=VECTOR('',#30721,10.);
#9174=VECTOR('',#30722,10.);
#9175=VECTOR('',#30725,10.);
#9176=VECTOR('',#30726,10.);
#9177=VECTOR('',#30727,10.);
#9178=VECTOR('',#30730,10.);
#9179=VECTOR('',#30731,10.);
#9180=VECTOR('',#30734,10.);
#9181=VECTOR('',#30735,10.);
#9182=VECTOR('',#30736,10.);
#9183=VECTOR('',#30737,10.);
#9184=VECTOR('',#30738,10.);
#9185=VECTOR('',#30741,10.);
#9186=VECTOR('',#30742,10.);
#9187=VECTOR('',#30743,10.);
#9188=VECTOR('',#30746,10.);
#9189=VECTOR('',#30747,10.);
#9190=VECTOR('',#30750,10.);
#9191=VECTOR('',#30751,10.);
#9192=VECTOR('',#30752,10.);
#9193=VECTOR('',#30753,10.);
#9194=VECTOR('',#30754,10.);
#9195=VECTOR('',#30757,10.);
#9196=VECTOR('',#30758,10.);
#9197=VECTOR('',#30759,10.);
#9198=VECTOR('',#30762,10.);
#9199=VECTOR('',#30763,10.);
#9200=VECTOR('',#30766,10.);
#9201=VECTOR('',#30767,10.);
#9202=VECTOR('',#30768,10.);
#9203=VECTOR('',#30769,10.);
#9204=VECTOR('',#30770,10.);
#9205=VECTOR('',#30773,10.);
#9206=VECTOR('',#30774,10.);
#9207=VECTOR('',#30775,10.);
#9208=VECTOR('',#30778,10.);
#9209=VECTOR('',#30779,10.);
#9210=VECTOR('',#30782,10.);
#9211=VECTOR('',#30783,10.);
#9212=VECTOR('',#30784,10.);
#9213=VECTOR('',#30785,10.);
#9214=VECTOR('',#30786,10.);
#9215=VECTOR('',#30789,10.);
#9216=VECTOR('',#30790,10.);
#9217=VECTOR('',#30791,10.);
#9218=VECTOR('',#30794,10.);
#9219=VECTOR('',#30795,10.);
#9220=VECTOR('',#30798,10.);
#9221=VECTOR('',#30799,10.);
#9222=VECTOR('',#30800,10.);
#9223=VECTOR('',#30801,10.);
#9224=VECTOR('',#30802,10.);
#9225=VECTOR('',#30805,10.);
#9226=VECTOR('',#30806,10.);
#9227=VECTOR('',#30807,10.);
#9228=VECTOR('',#30810,10.);
#9229=VECTOR('',#30811,10.);
#9230=VECTOR('',#30814,10.);
#9231=VECTOR('',#30815,10.);
#9232=VECTOR('',#30816,10.);
#9233=VECTOR('',#30817,10.);
#9234=VECTOR('',#30818,10.);
#9235=VECTOR('',#30821,10.);
#9236=VECTOR('',#30822,10.);
#9237=VECTOR('',#30823,10.);
#9238=VECTOR('',#30826,10.);
#9239=VECTOR('',#30827,10.);
#9240=VECTOR('',#30830,10.);
#9241=VECTOR('',#30831,10.);
#9242=VECTOR('',#30832,10.);
#9243=VECTOR('',#30833,10.);
#9244=VECTOR('',#30834,10.);
#9245=VECTOR('',#30837,10.);
#9246=VECTOR('',#30838,10.);
#9247=VECTOR('',#30839,10.);
#9248=VECTOR('',#30842,10.);
#9249=VECTOR('',#30843,10.);
#9250=VECTOR('',#30846,10.);
#9251=VECTOR('',#30847,10.);
#9252=VECTOR('',#30848,10.);
#9253=VECTOR('',#30849,10.);
#9254=VECTOR('',#30852,10.);
#9255=VECTOR('',#30853,10.);
#9256=VECTOR('',#30854,10.);
#9257=VECTOR('',#30855,10.);
#9258=VECTOR('',#30856,10.);
#9259=VECTOR('',#30857,10.);
#9260=VECTOR('',#30858,10.);
#9261=VECTOR('',#30859,10.);
#9262=VECTOR('',#30860,10.);
#9263=VECTOR('',#30861,10.);
#9264=VECTOR('',#30862,10.);
#9265=VECTOR('',#30863,10.);
#9266=VECTOR('',#30864,10.);
#9267=VECTOR('',#30865,10.);
#9268=VECTOR('',#30866,10.);
#9269=VECTOR('',#30867,10.);
#9270=VECTOR('',#30868,10.);
#9271=VECTOR('',#30869,10.);
#9272=VECTOR('',#30870,10.);
#9273=VECTOR('',#30871,10.);
#9274=VECTOR('',#30872,10.);
#9275=VECTOR('',#30873,10.);
#9276=VECTOR('',#30874,10.);
#9277=VECTOR('',#30875,10.);
#9278=VECTOR('',#30876,10.);
#9279=VECTOR('',#30877,10.);
#9280=VECTOR('',#30878,10.);
#9281=VECTOR('',#30879,10.);
#9282=VECTOR('',#30880,10.);
#9283=VECTOR('',#30881,10.);
#9284=VECTOR('',#30882,10.);
#9285=VECTOR('',#30883,10.);
#9286=VECTOR('',#30884,10.);
#9287=VECTOR('',#30885,10.);
#9288=VECTOR('',#30886,10.);
#9289=VECTOR('',#30887,10.);
#9290=VECTOR('',#30888,10.);
#9291=VECTOR('',#30889,10.);
#9292=VECTOR('',#30890,10.);
#9293=VECTOR('',#30891,10.);
#9294=VECTOR('',#30892,10.);
#9295=VECTOR('',#30893,10.);
#9296=VECTOR('',#30894,10.);
#9297=VECTOR('',#30895,10.);
#9298=VECTOR('',#30896,10.);
#9299=VECTOR('',#30897,10.);
#9300=VECTOR('',#30898,10.);
#9301=VECTOR('',#30899,10.);
#9302=VECTOR('',#30900,10.);
#9303=VECTOR('',#30901,10.);
#9304=VECTOR('',#30902,10.);
#9305=VECTOR('',#30903,10.);
#9306=VECTOR('',#30904,10.);
#9307=VECTOR('',#30905,10.);
#9308=VECTOR('',#30906,10.);
#9309=VECTOR('',#30907,10.);
#9310=VECTOR('',#30908,10.);
#9311=VECTOR('',#30909,10.);
#9312=VECTOR('',#30910,10.);
#9313=VECTOR('',#30911,10.);
#9314=VECTOR('',#30912,10.);
#9315=VECTOR('',#30913,10.);
#9316=VECTOR('',#30914,10.);
#9317=VECTOR('',#30915,10.);
#9318=VECTOR('',#30916,10.);
#9319=VECTOR('',#30917,10.);
#9320=VECTOR('',#30918,10.);
#9321=VECTOR('',#30919,10.);
#9322=VECTOR('',#30920,10.);
#9323=VECTOR('',#30921,10.);
#9324=VECTOR('',#30922,10.);
#9325=VECTOR('',#30923,10.);
#9326=VECTOR('',#30924,10.);
#9327=VECTOR('',#30925,10.);
#9328=VECTOR('',#30926,10.);
#9329=VECTOR('',#30927,10.);
#9330=VECTOR('',#30928,10.);
#9331=VECTOR('',#30929,10.);
#9332=VECTOR('',#30930,10.);
#9333=VECTOR('',#30931,10.);
#9334=VECTOR('',#30932,10.);
#9335=VECTOR('',#30933,10.);
#9336=VECTOR('',#30934,10.);
#9337=VECTOR('',#30935,10.);
#9338=VECTOR('',#30936,10.);
#9339=VECTOR('',#30937,10.);
#9340=VECTOR('',#30938,10.);
#9341=VECTOR('',#30939,10.);
#9342=VECTOR('',#30940,10.);
#9343=VECTOR('',#30941,10.);
#9344=VECTOR('',#30942,10.);
#9345=VECTOR('',#30943,10.);
#9346=VECTOR('',#30944,10.);
#9347=VECTOR('',#30945,10.);
#9348=VECTOR('',#30946,10.);
#9349=VECTOR('',#30947,10.);
#9350=VECTOR('',#30948,10.);
#9351=VECTOR('',#30949,10.);
#9352=VECTOR('',#30950,10.);
#9353=VECTOR('',#30951,10.);
#9354=VECTOR('',#30952,10.);
#9355=VECTOR('',#30953,10.);
#9356=VECTOR('',#30954,10.);
#9357=VECTOR('',#30955,10.);
#9358=VECTOR('',#30956,10.);
#9359=VECTOR('',#30957,10.);
#9360=VECTOR('',#30958,10.);
#9361=VECTOR('',#30959,10.);
#9362=VECTOR('',#30960,10.);
#9363=VECTOR('',#30961,10.);
#9364=VECTOR('',#30962,10.);
#9365=VECTOR('',#30963,10.);
#9366=VECTOR('',#30964,10.);
#9367=VECTOR('',#30965,10.);
#9368=VECTOR('',#30966,10.);
#9369=VECTOR('',#30967,10.);
#9370=VECTOR('',#30968,10.);
#9371=VECTOR('',#30969,10.);
#9372=VECTOR('',#30970,10.);
#9373=VECTOR('',#30971,10.);
#9374=VECTOR('',#30972,10.);
#9375=VECTOR('',#30973,10.);
#9376=VECTOR('',#30974,10.);
#9377=VECTOR('',#30975,10.);
#9378=VECTOR('',#30976,10.);
#9379=VECTOR('',#30977,10.);
#9380=VECTOR('',#30978,10.);
#9381=VECTOR('',#30979,10.);
#9382=VECTOR('',#30980,10.);
#9383=VECTOR('',#30981,10.);
#9384=VECTOR('',#30982,10.);
#9385=VECTOR('',#30983,10.);
#9386=VECTOR('',#30984,10.);
#9387=VECTOR('',#30985,10.);
#9388=VECTOR('',#30986,10.);
#9389=VECTOR('',#30987,10.);
#9390=VECTOR('',#30988,10.);
#9391=VECTOR('',#30989,10.);
#9392=VECTOR('',#30990,10.);
#9393=VECTOR('',#30991,10.);
#9394=VECTOR('',#30992,10.);
#9395=VECTOR('',#30993,10.);
#9396=VECTOR('',#30994,10.);
#9397=VECTOR('',#30995,10.);
#9398=VECTOR('',#30996,10.);
#9399=VECTOR('',#30997,10.);
#9400=VECTOR('',#30998,10.);
#9401=VECTOR('',#30999,10.);
#9402=VECTOR('',#31000,10.);
#9403=VECTOR('',#31001,10.);
#9404=VECTOR('',#31002,10.);
#9405=VECTOR('',#31003,10.);
#9406=VECTOR('',#31004,10.);
#9407=VECTOR('',#31005,10.);
#9408=VECTOR('',#31006,10.);
#9409=VECTOR('',#31007,10.);
#9410=VECTOR('',#31008,10.);
#9411=VECTOR('',#31009,10.);
#9412=VECTOR('',#31010,10.);
#9413=VECTOR('',#31011,10.);
#9414=VECTOR('',#31012,10.);
#9415=VECTOR('',#31013,10.);
#9416=VECTOR('',#31014,10.);
#9417=VECTOR('',#31015,10.);
#9418=VECTOR('',#31016,10.);
#9419=VECTOR('',#31017,10.);
#9420=VECTOR('',#31018,10.);
#9421=VECTOR('',#31019,10.);
#9422=VECTOR('',#31020,10.);
#9423=VECTOR('',#31021,10.);
#9424=VECTOR('',#31022,10.);
#9425=VECTOR('',#31023,10.);
#9426=VECTOR('',#31024,10.);
#9427=VECTOR('',#31025,10.);
#9428=VECTOR('',#31026,10.);
#9429=VECTOR('',#31027,10.);
#9430=VECTOR('',#31028,10.);
#9431=VECTOR('',#31029,10.);
#9432=VECTOR('',#31030,10.);
#9433=VECTOR('',#31031,10.);
#9434=VECTOR('',#31032,10.);
#9435=VECTOR('',#31033,10.);
#9436=VECTOR('',#31034,10.);
#9437=VECTOR('',#31035,10.);
#9438=VECTOR('',#31036,10.);
#9439=VECTOR('',#31037,10.);
#9440=VECTOR('',#31038,10.);
#9441=VECTOR('',#31039,10.);
#9442=VECTOR('',#31040,10.);
#9443=VECTOR('',#31041,10.);
#9444=VECTOR('',#31042,10.);
#9445=VECTOR('',#31043,10.);
#9446=VECTOR('',#31044,10.);
#9447=VECTOR('',#31045,10.);
#9448=VECTOR('',#31046,10.);
#9449=VECTOR('',#31047,10.);
#9450=VECTOR('',#31048,10.);
#9451=VECTOR('',#31049,10.);
#9452=VECTOR('',#31050,10.);
#9453=VECTOR('',#31051,10.);
#9454=VECTOR('',#31052,10.);
#9455=VECTOR('',#31053,10.);
#9456=VECTOR('',#31054,10.);
#9457=VECTOR('',#31055,10.);
#9458=VECTOR('',#31056,10.);
#9459=VECTOR('',#31057,10.);
#9460=VECTOR('',#31058,10.);
#9461=VECTOR('',#31059,10.);
#9462=VECTOR('',#31060,10.);
#9463=VECTOR('',#31061,10.);
#9464=VECTOR('',#31062,10.);
#9465=VECTOR('',#31063,10.);
#9466=VECTOR('',#31064,10.);
#9467=VECTOR('',#31065,10.);
#9468=VECTOR('',#31066,10.);
#9469=VECTOR('',#31067,10.);
#9470=VECTOR('',#31068,10.);
#9471=VECTOR('',#31069,10.);
#9472=VECTOR('',#31070,10.);
#9473=VECTOR('',#31071,10.);
#9474=VECTOR('',#31072,10.);
#9475=VECTOR('',#31073,10.);
#9476=VECTOR('',#31074,10.);
#9477=VECTOR('',#31075,10.);
#9478=VECTOR('',#31076,10.);
#9479=VECTOR('',#31077,10.);
#9480=VECTOR('',#31078,10.);
#9481=VECTOR('',#31083,10.);
#9482=VECTOR('',#31084,10.);
#9483=VECTOR('',#31085,10.);
#9484=VECTOR('',#31088,10.);
#9485=VECTOR('',#31089,10.);
#9486=VECTOR('',#31090,10.);
#9487=VECTOR('',#31093,10.);
#9488=VECTOR('',#31094,10.);
#9489=VECTOR('',#31095,10.);
#9490=VECTOR('',#31098,10.);
#9491=VECTOR('',#31099,10.);
#9492=VECTOR('',#31100,10.);
#9493=VECTOR('',#31103,10.);
#9494=VECTOR('',#31104,10.);
#9495=VECTOR('',#31105,10.);
#9496=VECTOR('',#31108,10.);
#9497=VECTOR('',#31109,10.);
#9498=VECTOR('',#31110,10.);
#9499=VECTOR('',#31113,10.);
#9500=VECTOR('',#31114,10.);
#9501=VECTOR('',#31115,10.);
#9502=VECTOR('',#31118,10.);
#9503=VECTOR('',#31119,10.);
#9504=VECTOR('',#31120,10.);
#9505=VECTOR('',#31123,10.);
#9506=VECTOR('',#31124,10.);
#9507=VECTOR('',#31125,10.);
#9508=VECTOR('',#31128,10.);
#9509=VECTOR('',#31129,10.);
#9510=VECTOR('',#31130,10.);
#9511=VECTOR('',#31133,10.);
#9512=VECTOR('',#31134,10.);
#9513=VECTOR('',#31135,10.);
#9514=VECTOR('',#31138,10.);
#9515=VECTOR('',#31139,10.);
#9516=VECTOR('',#31140,10.);
#9517=VECTOR('',#31143,10.);
#9518=VECTOR('',#31144,10.);
#9519=VECTOR('',#31145,10.);
#9520=VECTOR('',#31148,10.);
#9521=VECTOR('',#31149,10.);
#9522=VECTOR('',#31150,10.);
#9523=VECTOR('',#31153,10.);
#9524=VECTOR('',#31154,10.);
#9525=VECTOR('',#31155,10.);
#9526=VECTOR('',#31158,10.);
#9527=VECTOR('',#31159,10.);
#9528=VECTOR('',#31160,10.);
#9529=VECTOR('',#31163,10.);
#9530=VECTOR('',#31164,10.);
#9531=VECTOR('',#31165,10.);
#9532=VECTOR('',#31168,10.);
#9533=VECTOR('',#31169,10.);
#9534=VECTOR('',#31170,10.);
#9535=VECTOR('',#31173,10.);
#9536=VECTOR('',#31174,10.);
#9537=VECTOR('',#31175,10.);
#9538=VECTOR('',#31178,10.);
#9539=VECTOR('',#31179,10.);
#9540=VECTOR('',#31180,10.);
#9541=VECTOR('',#31183,10.);
#9542=VECTOR('',#31184,10.);
#9543=VECTOR('',#31185,10.);
#9544=VECTOR('',#31188,10.);
#9545=VECTOR('',#31189,10.);
#9546=VECTOR('',#31190,10.);
#9547=VECTOR('',#31193,10.);
#9548=VECTOR('',#31194,10.);
#9549=VECTOR('',#31195,10.);
#9550=VECTOR('',#31198,10.);
#9551=VECTOR('',#31199,10.);
#9552=VECTOR('',#31202,10.);
#9553=VECTOR('',#31207,10.);
#9554=VECTOR('',#31210,10.);
#9555=VECTOR('',#31213,10.);
#9556=VECTOR('',#31216,10.);
#9557=VECTOR('',#31219,10.);
#9558=VECTOR('',#31222,10.);
#9559=VECTOR('',#31225,10.);
#9560=VECTOR('',#31228,10.);
#9561=VECTOR('',#31231,10.);
#9562=VECTOR('',#31234,10.);
#9563=VECTOR('',#31237,10.);
#9564=VECTOR('',#31240,10.);
#9565=VECTOR('',#31243,10.);
#9566=VECTOR('',#31246,10.);
#9567=VECTOR('',#31249,10.);
#9568=VECTOR('',#31254,10.);
#9569=VECTOR('',#31257,10.);
#9570=VECTOR('',#31260,10.);
#9571=VECTOR('',#31265,10.);
#9572=VECTOR('',#31268,10.);
#9573=VECTOR('',#31271,10.);
#9574=VECTOR('',#31274,10.);
#9575=VECTOR('',#31277,10.);
#9576=VECTOR('',#31280,10.);
#9577=VECTOR('',#31283,10.);
#9578=VECTOR('',#31286,10.);
#9579=VECTOR('',#31289,10.);
#9580=VECTOR('',#31292,10.);
#9581=VECTOR('',#31295,10.);
#9582=VECTOR('',#31298,10.);
#9583=VECTOR('',#31301,10.);
#9584=VECTOR('',#31304,10.);
#9585=VECTOR('',#31307,10.);
#9586=VECTOR('',#31312,10.);
#9587=VECTOR('',#31315,10.);
#9588=VECTOR('',#31318,10.);
#9589=VECTOR('',#31323,10.);
#9590=VECTOR('',#31326,10.);
#9591=VECTOR('',#31329,10.);
#9592=VECTOR('',#31332,10.);
#9593=VECTOR('',#31335,10.);
#9594=VECTOR('',#31338,10.);
#9595=VECTOR('',#31341,10.);
#9596=VECTOR('',#31344,10.);
#9597=VECTOR('',#31347,10.);
#9598=VECTOR('',#31350,10.);
#9599=VECTOR('',#31353,10.);
#9600=VECTOR('',#31356,10.);
#9601=VECTOR('',#31359,10.);
#9602=VECTOR('',#31362,10.);
#9603=VECTOR('',#31365,10.);
#9604=VECTOR('',#31370,10.);
#9605=VECTOR('',#31373,10.);
#9606=VECTOR('',#31376,10.);
#9607=VECTOR('',#31381,10.);
#9608=VECTOR('',#31384,10.);
#9609=VECTOR('',#31387,10.);
#9610=VECTOR('',#31390,10.);
#9611=VECTOR('',#31393,10.);
#9612=VECTOR('',#31396,10.);
#9613=VECTOR('',#31399,10.);
#9614=VECTOR('',#31402,10.);
#9615=VECTOR('',#31405,10.);
#9616=VECTOR('',#31408,10.);
#9617=VECTOR('',#31411,10.);
#9618=VECTOR('',#31414,10.);
#9619=VECTOR('',#31417,10.);
#9620=VECTOR('',#31420,10.);
#9621=VECTOR('',#31423,10.);
#9622=VECTOR('',#31428,10.);
#9623=VECTOR('',#31431,10.);
#9624=VECTOR('',#31434,10.);
#9625=VECTOR('',#31439,10.);
#9626=VECTOR('',#31442,10.);
#9627=VECTOR('',#31445,10.);
#9628=VECTOR('',#31448,10.);
#9629=VECTOR('',#31451,10.);
#9630=VECTOR('',#31454,10.);
#9631=VECTOR('',#31457,10.);
#9632=VECTOR('',#31460,10.);
#9633=VECTOR('',#31463,10.);
#9634=VECTOR('',#31466,10.);
#9635=VECTOR('',#31469,10.);
#9636=VECTOR('',#31472,10.);
#9637=VECTOR('',#31475,10.);
#9638=VECTOR('',#31478,10.);
#9639=VECTOR('',#31481,10.);
#9640=VECTOR('',#31486,10.);
#9641=VECTOR('',#31489,10.);
#9642=VECTOR('',#31492,10.);
#9643=VECTOR('',#31497,10.);
#9644=VECTOR('',#31500,10.);
#9645=VECTOR('',#31503,10.);
#9646=VECTOR('',#31506,10.);
#9647=VECTOR('',#31509,10.);
#9648=VECTOR('',#31512,10.);
#9649=VECTOR('',#31515,10.);
#9650=VECTOR('',#31518,10.);
#9651=VECTOR('',#31521,10.);
#9652=VECTOR('',#31524,10.);
#9653=VECTOR('',#31527,10.);
#9654=VECTOR('',#31530,10.);
#9655=VECTOR('',#31533,10.);
#9656=VECTOR('',#31536,10.);
#9657=VECTOR('',#31539,10.);
#9658=VECTOR('',#31544,10.);
#9659=VECTOR('',#31547,10.);
#9660=VECTOR('',#31550,10.);
#9661=VECTOR('',#31555,10.);
#9662=VECTOR('',#31558,10.);
#9663=VECTOR('',#31561,10.);
#9664=VECTOR('',#31564,10.);
#9665=VECTOR('',#31567,10.);
#9666=VECTOR('',#31570,10.);
#9667=VECTOR('',#31573,10.);
#9668=VECTOR('',#31576,10.);
#9669=VECTOR('',#31579,10.);
#9670=VECTOR('',#31582,10.);
#9671=VECTOR('',#31585,10.);
#9672=VECTOR('',#31588,10.);
#9673=VECTOR('',#31591,10.);
#9674=VECTOR('',#31594,10.);
#9675=VECTOR('',#31597,10.);
#9676=VECTOR('',#31602,10.);
#9677=VECTOR('',#31605,10.);
#9678=VECTOR('',#31608,10.);
#9679=VECTOR('',#31613,10.);
#9680=VECTOR('',#31616,10.);
#9681=VECTOR('',#31619,10.);
#9682=VECTOR('',#31622,10.);
#9683=VECTOR('',#31625,10.);
#9684=VECTOR('',#31628,10.);
#9685=VECTOR('',#31631,10.);
#9686=VECTOR('',#31634,10.);
#9687=VECTOR('',#31637,10.);
#9688=VECTOR('',#31640,10.);
#9689=VECTOR('',#31643,10.);
#9690=VECTOR('',#31646,10.);
#9691=VECTOR('',#31649,10.);
#9692=VECTOR('',#31652,10.);
#9693=VECTOR('',#31655,10.);
#9694=VECTOR('',#31660,10.);
#9695=VECTOR('',#31663,10.);
#9696=VECTOR('',#31666,10.);
#9697=VECTOR('',#31671,10.);
#9698=VECTOR('',#31674,10.);
#9699=VECTOR('',#31677,10.);
#9700=VECTOR('',#31680,10.);
#9701=VECTOR('',#31683,10.);
#9702=VECTOR('',#31686,10.);
#9703=VECTOR('',#31689,10.);
#9704=VECTOR('',#31692,10.);
#9705=VECTOR('',#31695,10.);
#9706=VECTOR('',#31698,10.);
#9707=VECTOR('',#31701,10.);
#9708=VECTOR('',#31704,10.);
#9709=VECTOR('',#31707,10.);
#9710=VECTOR('',#31710,10.);
#9711=VECTOR('',#31713,10.);
#9712=VECTOR('',#31718,10.);
#9713=VECTOR('',#31721,10.);
#9714=VECTOR('',#31724,10.);
#9715=VECTOR('',#31729,10.);
#9716=VECTOR('',#31732,10.);
#9717=VECTOR('',#31735,10.);
#9718=VECTOR('',#31738,10.);
#9719=VECTOR('',#31741,10.);
#9720=VECTOR('',#31744,10.);
#9721=VECTOR('',#31747,10.);
#9722=VECTOR('',#31750,10.);
#9723=VECTOR('',#31753,10.);
#9724=VECTOR('',#31756,10.);
#9725=VECTOR('',#31759,10.);
#9726=VECTOR('',#31762,10.);
#9727=VECTOR('',#31765,10.);
#9728=VECTOR('',#31768,10.);
#9729=VECTOR('',#31771,10.);
#9730=VECTOR('',#31776,10.);
#9731=VECTOR('',#31779,10.);
#9732=VECTOR('',#31782,10.);
#9733=VECTOR('',#31787,10.);
#9734=VECTOR('',#31790,10.);
#9735=VECTOR('',#31793,10.);
#9736=VECTOR('',#31796,10.);
#9737=VECTOR('',#31799,10.);
#9738=VECTOR('',#31802,10.);
#9739=VECTOR('',#31805,10.);
#9740=VECTOR('',#31808,10.);
#9741=VECTOR('',#31811,10.);
#9742=VECTOR('',#31814,10.);
#9743=VECTOR('',#31817,10.);
#9744=VECTOR('',#31820,10.);
#9745=VECTOR('',#31823,10.);
#9746=VECTOR('',#31826,10.);
#9747=VECTOR('',#31829,10.);
#9748=VECTOR('',#31834,10.);
#9749=VECTOR('',#31837,10.);
#9750=VECTOR('',#31840,10.);
#9751=VECTOR('',#31845,10.);
#9752=VECTOR('',#31848,10.);
#9753=VECTOR('',#31851,10.);
#9754=VECTOR('',#31854,10.);
#9755=VECTOR('',#31857,10.);
#9756=VECTOR('',#31860,10.);
#9757=VECTOR('',#31863,10.);
#9758=VECTOR('',#31866,10.);
#9759=VECTOR('',#31869,10.);
#9760=VECTOR('',#31872,10.);
#9761=VECTOR('',#31875,10.);
#9762=VECTOR('',#31878,10.);
#9763=VECTOR('',#31881,10.);
#9764=VECTOR('',#31884,10.);
#9765=VECTOR('',#31887,10.);
#9766=VECTOR('',#31894,8.5);
#9767=VECTOR('',#31903,8.5);
#9768=VECTOR('',#31910,10.);
#9769=VECTOR('',#31911,10.);
#9770=VECTOR('',#31912,10.);
#9771=VECTOR('',#31913,10.);
#9772=VECTOR('',#31916,10.);
#9773=VECTOR('',#31917,10.);
#9774=VECTOR('',#31918,10.);
#9775=VECTOR('',#31921,10.);
#9776=VECTOR('',#31922,10.);
#9777=VECTOR('',#31923,10.);
#9778=VECTOR('',#31926,10.);
#9779=VECTOR('',#31927,10.);
#9780=VECTOR('',#31932,10.);
#9781=VECTOR('',#31933,10.);
#9782=VECTOR('',#31934,10.);
#9783=VECTOR('',#31935,10.);
#9784=VECTOR('',#31938,10.);
#9785=VECTOR('',#31939,10.);
#9786=VECTOR('',#31940,10.);
#9787=VECTOR('',#31943,10.);
#9788=VECTOR('',#31944,10.);
#9789=VECTOR('',#31945,10.);
#9790=VECTOR('',#31948,10.);
#9791=VECTOR('',#31949,10.);
#9792=VECTOR('',#31956,11.5);
#9793=VECTOR('',#31963,11.5);
#9794=VECTOR('',#31970,10.);
#9795=VECTOR('',#31973,10.);
#9796=VECTOR('',#31992,9.47407799863808);
#9797=VECTOR('',#32003,10.15);
#9798=VECTOR('',#32008,7.94);
#9799=VECTOR('',#32017,14.29);
#9800=VECTOR('',#32024,12.);
#9801=VECTOR('',#32033,9.07);
#9802=VECTOR('',#32038,10.);
#9803=VECTOR('',#32041,10.);
#9804=VECTOR('',#32050,10.);
#9805=VECTOR('',#32053,10.);
#9806=VECTOR('',#32056,10.);
#9807=VECTOR('',#32057,10.);
#9808=VECTOR('',#32058,10.);
#9809=VECTOR('',#32061,10.);
#9810=VECTOR('',#32066,10.);
#9811=VECTOR('',#32067,10.);
#9812=VECTOR('',#32072,10.);
#9813=VECTOR('',#32079,10.);
#9814=VECTOR('',#32096,0.900000000000001);
#9815=VECTOR('',#32101,0.800000000000001);
#9816=VECTOR('',#32108,0.900000000000001);
#9817=VECTOR('',#32115,0.900000000000001);
#9818=VECTOR('',#32120,0.800000000000001);
#9819=VECTOR('',#32125,0.900000000000001);
#9820=VECTOR('',#32130,10.);
#9821=VECTOR('',#32131,10.);
#9822=VECTOR('',#32132,10.);
#9823=VECTOR('',#32133,10.);
#9824=VECTOR('',#32134,10.);
#9825=VECTOR('',#32135,10.);
#9826=VECTOR('',#32138,10.);
#9827=VECTOR('',#32139,10.);
#9828=VECTOR('',#32140,10.);
#9829=VECTOR('',#32143,10.);
#9830=VECTOR('',#32144,10.);
#9831=VECTOR('',#32145,10.);
#9832=VECTOR('',#32146,10.);
#9833=VECTOR('',#32149,10.);
#9834=VECTOR('',#32150,10.);
#9835=VECTOR('',#32151,10.);
#9836=VECTOR('',#32152,10.);
#9837=VECTOR('',#32155,10.);
#9838=VECTOR('',#32156,10.);
#9839=VECTOR('',#32157,10.);
#9840=VECTOR('',#32158,10.);
#9841=VECTOR('',#32159,10.);
#9842=VECTOR('',#32162,10.);
#9843=VECTOR('',#32163,10.);
#9844=VECTOR('',#32164,10.);
#9845=VECTOR('',#32167,10.);
#9846=VECTOR('',#32168,10.);
#9847=VECTOR('',#32169,10.);
#9848=VECTOR('',#32170,10.);
#9849=VECTOR('',#32173,10.);
#9850=VECTOR('',#32174,10.);
#9851=VECTOR('',#32175,10.);
#9852=VECTOR('',#32178,10.);
#9853=VECTOR('',#32179,10.);
#9854=VECTOR('',#32182,10.);
#9855=VECTOR('',#32183,10.);
#9856=VECTOR('',#32184,10.);
#9857=VECTOR('',#32185,10.);
#9858=VECTOR('',#32188,10.);
#9859=VECTOR('',#32189,10.);
#9860=VECTOR('',#32190,10.);
#9861=VECTOR('',#32193,10.);
#9862=VECTOR('',#32194,10.);
#9863=VECTOR('',#32197,10.);
#9864=VECTOR('',#32198,10.);
#9865=VECTOR('',#32199,10.);
#9866=VECTOR('',#32202,10.);
#9867=VECTOR('',#32205,10.);
#9868=VECTOR('',#32228,1.);
#9869=VECTOR('',#32243,1.);
#9870=VECTOR('',#32248,10.);
#9871=VECTOR('',#32249,10.);
#9872=VECTOR('',#32250,10.);
#9873=VECTOR('',#32253,10.);
#9874=VECTOR('',#32254,10.);
#9875=VECTOR('',#32255,10.);
#9876=VECTOR('',#32258,10.);
#9877=VECTOR('',#32259,10.);
#9878=VECTOR('',#32260,10.);
#9879=VECTOR('',#32263,10.);
#9880=VECTOR('',#32264,10.);
#9881=VECTOR('',#32265,10.);
#9882=VECTOR('',#32268,10.);
#9883=VECTOR('',#32269,10.);
#9884=VECTOR('',#32272,10.);
#9885=VECTOR('',#32273,10.);
#9886=VECTOR('',#32274,10.);
#9887=VECTOR('',#32277,10.);
#9888=VECTOR('',#32278,10.);
#9889=VECTOR('',#32279,10.);
#9890=VECTOR('',#32282,10.);
#9891=VECTOR('',#32283,10.);
#9892=VECTOR('',#32286,10.);
#9893=VECTOR('',#32287,10.);
#9894=VECTOR('',#32290,10.);
#9895=VECTOR('',#32291,10.);
#9896=VECTOR('',#32294,10.);
#9897=VECTOR('',#32295,10.);
#9898=VECTOR('',#32298,10.);
#9899=VECTOR('',#32299,10.);
#9900=VECTOR('',#32302,10.);
#9901=VECTOR('',#32303,10.);
#9902=VECTOR('',#32306,10.);
#9903=VECTOR('',#32307,10.);
#9904=VECTOR('',#32310,10.);
#9905=VECTOR('',#32311,10.);
#9906=VECTOR('',#32314,10.);
#9907=VECTOR('',#32315,10.);
#9908=VECTOR('',#32318,10.);
#9909=VECTOR('',#32319,10.);
#9910=VECTOR('',#32322,10.);
#9911=VECTOR('',#32323,10.);
#9912=VECTOR('',#32336,10.);
#9913=VECTOR('',#32337,10.);
#9914=VECTOR('',#32338,10.);
#9915=VECTOR('',#32339,10.);
#9916=VECTOR('',#32342,10.);
#9917=VECTOR('',#32343,10.);
#9918=VECTOR('',#32344,10.);
#9919=VECTOR('',#32347,10.);
#9920=VECTOR('',#32348,10.);
#9921=VECTOR('',#32349,10.);
#9922=VECTOR('',#32350,10.);
#9923=VECTOR('',#32353,10.);
#9924=VECTOR('',#32354,10.);
#9925=VECTOR('',#32355,10.);
#9926=VECTOR('',#32358,10.);
#9927=VECTOR('',#32359,10.);
#9928=VECTOR('',#32362,10.);
#9929=VECTOR('',#32363,10.);
#9930=VECTOR('',#32366,10.);
#9931=VECTOR('',#32367,10.);
#9932=VECTOR('',#32368,10.);
#9933=VECTOR('',#32371,10.);
#9934=VECTOR('',#32372,10.);
#9935=VECTOR('',#32375,10.);
#9936=VECTOR('',#32376,10.);
#9937=VECTOR('',#32383,10.);
#9938=VECTOR('',#32384,10.);
#9939=VECTOR('',#32387,10.);
#9940=VECTOR('',#32388,10.);
#9941=VECTOR('',#32391,10.);
#9942=VECTOR('',#32396,9.4);
#9943=VECTOR('',#32411,6.89);
#9944=VECTOR('',#32416,7.14);
#9945=VECTOR('',#32423,6.2);
#9946=VECTOR('',#32430,8.5);
#9947=VECTOR('',#32445,10.7);
#9948=VECTOR('',#32450,9.);
#9949=VECTOR('',#32461,11.5);
#9950=VECTOR('',#32468,9.);
#9951=VECTOR('',#32475,10.7);
#9952=VECTOR('',#32484,5.);
#9953=VECTOR('',#32489,5.);
#9954=VECTOR('',#32492,5.);
#9955=VECTOR('',#32495,5.);
#9956=VECTOR('',#32498,5.);
#9957=VECTOR('',#32501,5.);
#9958=VECTOR('',#32504,5.);
#9959=VECTOR('',#32507,5.);
#9960=VECTOR('',#32510,5.);
#9961=VECTOR('',#32513,5.);
#9962=VECTOR('',#32516,5.);
#9963=VECTOR('',#32519,5.);
#9964=VECTOR('',#32522,5.);
#9965=VECTOR('',#32525,5.);
#9966=VECTOR('',#32528,5.);
#9967=VECTOR('',#32531,5.);
#9968=VECTOR('',#32534,5.);
#9969=VECTOR('',#32537,5.);
#9970=VECTOR('',#32540,5.);
#9971=VECTOR('',#32543,5.);
#9972=VECTOR('',#32546,5.);
#9973=VECTOR('',#32551,4.0705);
#9974=VECTOR('',#32556,4.0705);
#9975=VECTOR('',#32559,4.0705);
#9976=VECTOR('',#32562,4.0705);
#9977=VECTOR('',#32565,4.0705);
#9978=VECTOR('',#32568,4.0705);
#9979=VECTOR('',#32571,4.0705);
#9980=VECTOR('',#32574,4.0705);
#9981=VECTOR('',#32577,4.0705);
#9982=VECTOR('',#32580,4.0705);
#9983=VECTOR('',#32583,4.0705);
#9984=VECTOR('',#32586,4.0705);
#9985=VECTOR('',#32589,4.0705);
#9986=VECTOR('',#32592,4.0705);
#9987=VECTOR('',#32595,4.0705);
#9988=VECTOR('',#32598,4.0705);
#9989=VECTOR('',#32601,4.0705);
#9990=VECTOR('',#32604,4.0705);
#9991=VECTOR('',#32607,4.0705);
#9992=VECTOR('',#32610,4.0705);
#9993=VECTOR('',#32627,10.);
#9994=VECTOR('',#32628,10.);
#9995=VECTOR('',#32629,10.);
#9996=VECTOR('',#32630,10.);
#9997=VECTOR('',#32635,10.);
#9998=VECTOR('',#32638,10.);
#9999=VECTOR('',#32639,10.);
#10000=VECTOR('',#32646,10.);
#10001=VECTOR('',#32647,10.);
#10002=VECTOR('',#32648,10.);
#10003=VECTOR('',#32649,10.);
#10004=VECTOR('',#32654,10.);
#10005=VECTOR('',#32657,10.);
#10006=VECTOR('',#32658,10.);
#10007=VECTOR('',#32665,10.);
#10008=VECTOR('',#32666,10.);
#10009=VECTOR('',#32667,10.);
#10010=VECTOR('',#32668,10.);
#10011=VECTOR('',#32673,10.);
#10012=VECTOR('',#32676,10.);
#10013=VECTOR('',#32677,10.);
#10014=VECTOR('',#32684,10.);
#10015=VECTOR('',#32685,10.);
#10016=VECTOR('',#32686,10.);
#10017=VECTOR('',#32687,10.);
#10018=VECTOR('',#32692,10.);
#10019=VECTOR('',#32695,10.);
#10020=VECTOR('',#32696,10.);
#10021=VECTOR('',#32703,10.);
#10022=VECTOR('',#32704,10.);
#10023=VECTOR('',#32705,10.);
#10024=VECTOR('',#32706,10.);
#10025=VECTOR('',#32711,10.);
#10026=VECTOR('',#32714,10.);
#10027=VECTOR('',#32715,10.);
#10028=VECTOR('',#32722,10.);
#10029=VECTOR('',#32723,10.);
#10030=VECTOR('',#32724,10.);
#10031=VECTOR('',#32725,10.);
#10032=VECTOR('',#32730,10.);
#10033=VECTOR('',#32733,10.);
#10034=VECTOR('',#32734,10.);
#10035=VECTOR('',#32741,10.);
#10036=VECTOR('',#32742,10.);
#10037=VECTOR('',#32743,10.);
#10038=VECTOR('',#32744,10.);
#10039=VECTOR('',#32749,10.);
#10040=VECTOR('',#32752,10.);
#10041=VECTOR('',#32753,10.);
#10042=VECTOR('',#32760,10.);
#10043=VECTOR('',#32761,10.);
#10044=VECTOR('',#32762,10.);
#10045=VECTOR('',#32763,10.);
#10046=VECTOR('',#32768,10.);
#10047=VECTOR('',#32771,10.);
#10048=VECTOR('',#32772,10.);
#10049=VECTOR('',#32779,10.);
#10050=VECTOR('',#32780,10.);
#10051=VECTOR('',#32781,10.);
#10052=VECTOR('',#32782,10.);
#10053=VECTOR('',#32787,10.);
#10054=VECTOR('',#32790,10.);
#10055=VECTOR('',#32791,10.);
#10056=VECTOR('',#32798,10.);
#10057=VECTOR('',#32799,10.);
#10058=VECTOR('',#32800,10.);
#10059=VECTOR('',#32801,10.);
#10060=VECTOR('',#32806,10.);
#10061=VECTOR('',#32809,10.);
#10062=VECTOR('',#32810,10.);
#10063=VECTOR('',#32817,10.);
#10064=VECTOR('',#32818,10.);
#10065=VECTOR('',#32819,10.);
#10066=VECTOR('',#32820,10.);
#10067=VECTOR('',#32825,10.);
#10068=VECTOR('',#32828,10.);
#10069=VECTOR('',#32829,10.);
#10070=VECTOR('',#32836,10.);
#10071=VECTOR('',#32837,10.);
#10072=VECTOR('',#32838,10.);
#10073=VECTOR('',#32839,10.);
#10074=VECTOR('',#32844,10.);
#10075=VECTOR('',#32847,10.);
#10076=VECTOR('',#32848,10.);
#10077=VECTOR('',#32855,10.);
#10078=VECTOR('',#32856,10.);
#10079=VECTOR('',#32857,10.);
#10080=VECTOR('',#32858,10.);
#10081=VECTOR('',#32863,10.);
#10082=VECTOR('',#32866,10.);
#10083=VECTOR('',#32867,10.);
#10084=VECTOR('',#32874,10.);
#10085=VECTOR('',#32875,10.);
#10086=VECTOR('',#32876,10.);
#10087=VECTOR('',#32877,10.);
#10088=VECTOR('',#32882,10.);
#10089=VECTOR('',#32885,10.);
#10090=VECTOR('',#32886,10.);
#10091=VECTOR('',#32893,10.);
#10092=VECTOR('',#32894,10.);
#10093=VECTOR('',#32895,10.);
#10094=VECTOR('',#32896,10.);
#10095=VECTOR('',#32901,10.);
#10096=VECTOR('',#32904,10.);
#10097=VECTOR('',#32905,10.);
#10098=VECTOR('',#32912,10.);
#10099=VECTOR('',#32913,10.);
#10100=VECTOR('',#32914,10.);
#10101=VECTOR('',#32915,10.);
#10102=VECTOR('',#32920,10.);
#10103=VECTOR('',#32923,10.);
#10104=VECTOR('',#32924,10.);
#10105=VECTOR('',#32931,10.);
#10106=VECTOR('',#32932,10.);
#10107=VECTOR('',#32933,10.);
#10108=VECTOR('',#32934,10.);
#10109=VECTOR('',#32939,10.);
#10110=VECTOR('',#32942,10.);
#10111=VECTOR('',#32943,10.);
#10112=VECTOR('',#32950,10.);
#10113=VECTOR('',#32951,10.);
#10114=VECTOR('',#32952,10.);
#10115=VECTOR('',#32953,10.);
#10116=VECTOR('',#32958,10.);
#10117=VECTOR('',#32963,10.);
#10118=VECTOR('',#32964,10.);
#10119=VECTOR('',#32973,10.);
#10120=VECTOR('',#32974,10.);
#10121=VECTOR('',#32975,10.);
#10122=VECTOR('',#32976,10.);
#10123=VECTOR('',#32981,10.);
#10124=VECTOR('',#32984,10.);
#10125=VECTOR('',#32985,10.);
#10126=VECTOR('',#32992,10.);
#10127=VECTOR('',#32993,10.);
#10128=VECTOR('',#32994,10.);
#10129=VECTOR('',#32995,10.);
#10130=VECTOR('',#33000,10.);
#10131=VECTOR('',#33003,10.);
#10132=VECTOR('',#33004,10.);
#10133=VECTOR('',#33011,10.);
#10134=VECTOR('',#33012,10.);
#10135=VECTOR('',#33013,10.);
#10136=VECTOR('',#33014,10.);
#10137=VECTOR('',#33019,10.);
#10138=VECTOR('',#33022,10.);
#10139=VECTOR('',#33023,10.);
#10140=VECTOR('',#33030,10.);
#10141=VECTOR('',#33031,10.);
#10142=VECTOR('',#33032,10.);
#10143=VECTOR('',#33033,10.);
#10144=VECTOR('',#33038,10.);
#10145=VECTOR('',#33041,10.);
#10146=VECTOR('',#33042,10.);
#10147=VECTOR('',#33049,10.);
#10148=VECTOR('',#33050,10.);
#10149=VECTOR('',#33051,10.);
#10150=VECTOR('',#33052,10.);
#10151=VECTOR('',#33057,10.);
#10152=VECTOR('',#33060,10.);
#10153=VECTOR('',#33061,10.);
#10154=VECTOR('',#33068,10.);
#10155=VECTOR('',#33069,10.);
#10156=VECTOR('',#33070,10.);
#10157=VECTOR('',#33071,10.);
#10158=VECTOR('',#33076,10.);
#10159=VECTOR('',#33079,10.);
#10160=VECTOR('',#33080,10.);
#10161=VECTOR('',#33087,10.);
#10162=VECTOR('',#33088,10.);
#10163=VECTOR('',#33089,10.);
#10164=VECTOR('',#33090,10.);
#10165=VECTOR('',#33095,10.);
#10166=VECTOR('',#33098,10.);
#10167=VECTOR('',#33099,10.);
#10168=VECTOR('',#33106,10.);
#10169=VECTOR('',#33107,10.);
#10170=VECTOR('',#33108,10.);
#10171=VECTOR('',#33109,10.);
#10172=VECTOR('',#33114,10.);
#10173=VECTOR('',#33117,10.);
#10174=VECTOR('',#33118,10.);
#10175=VECTOR('',#33125,10.);
#10176=VECTOR('',#33126,10.);
#10177=VECTOR('',#33127,10.);
#10178=VECTOR('',#33128,10.);
#10179=VECTOR('',#33133,10.);
#10180=VECTOR('',#33136,10.);
#10181=VECTOR('',#33137,10.);
#10182=VECTOR('',#33144,10.);
#10183=VECTOR('',#33145,10.);
#10184=VECTOR('',#33146,10.);
#10185=VECTOR('',#33147,10.);
#10186=VECTOR('',#33152,10.);
#10187=VECTOR('',#33155,10.);
#10188=VECTOR('',#33156,10.);
#10189=VECTOR('',#33163,10.);
#10190=VECTOR('',#33164,10.);
#10191=VECTOR('',#33165,10.);
#10192=VECTOR('',#33166,10.);
#10193=VECTOR('',#33171,10.);
#10194=VECTOR('',#33174,10.);
#10195=VECTOR('',#33175,10.);
#10196=VECTOR('',#33182,10.);
#10197=VECTOR('',#33183,10.);
#10198=VECTOR('',#33184,10.);
#10199=VECTOR('',#33185,10.);
#10200=VECTOR('',#33190,10.);
#10201=VECTOR('',#33193,10.);
#10202=VECTOR('',#33194,10.);
#10203=VECTOR('',#33201,10.);
#10204=VECTOR('',#33202,10.);
#10205=VECTOR('',#33203,10.);
#10206=VECTOR('',#33204,10.);
#10207=VECTOR('',#33209,10.);
#10208=VECTOR('',#33212,10.);
#10209=VECTOR('',#33213,10.);
#10210=VECTOR('',#33220,10.);
#10211=VECTOR('',#33221,10.);
#10212=VECTOR('',#33222,10.);
#10213=VECTOR('',#33223,10.);
#10214=VECTOR('',#33228,10.);
#10215=VECTOR('',#33231,10.);
#10216=VECTOR('',#33232,10.);
#10217=VECTOR('',#33239,10.);
#10218=VECTOR('',#33240,10.);
#10219=VECTOR('',#33241,10.);
#10220=VECTOR('',#33242,10.);
#10221=VECTOR('',#33247,10.);
#10222=VECTOR('',#33250,10.);
#10223=VECTOR('',#33251,10.);
#10224=VECTOR('',#33258,10.);
#10225=VECTOR('',#33259,10.);
#10226=VECTOR('',#33260,10.);
#10227=VECTOR('',#33261,10.);
#10228=VECTOR('',#33266,10.);
#10229=VECTOR('',#33269,10.);
#10230=VECTOR('',#33270,10.);
#10231=VECTOR('',#33277,10.);
#10232=VECTOR('',#33278,10.);
#10233=VECTOR('',#33279,10.);
#10234=VECTOR('',#33280,10.);
#10235=VECTOR('',#33285,10.);
#10236=VECTOR('',#33288,10.);
#10237=VECTOR('',#33289,10.);
#10238=VECTOR('',#33296,10.);
#10239=VECTOR('',#33297,10.);
#10240=VECTOR('',#33298,10.);
#10241=VECTOR('',#33299,10.);
#10242=VECTOR('',#33304,10.);
#10243=VECTOR('',#33307,10.);
#10244=VECTOR('',#33308,10.);
#10245=VECTOR('',#33315,10.);
#10246=VECTOR('',#33316,10.);
#10247=VECTOR('',#33317,10.);
#10248=VECTOR('',#33318,10.);
#10249=VECTOR('',#33321,10.);
#10250=VECTOR('',#33322,10.);
#10251=VECTOR('',#33323,10.);
#10252=VECTOR('',#33326,10.);
#10253=VECTOR('',#33327,10.);
#10254=VECTOR('',#33328,10.);
#10255=VECTOR('',#33331,10.);
#10256=VECTOR('',#33332,10.);
#10257=VECTOR('',#33333,10.);
#10258=VECTOR('',#33336,10.);
#10259=VECTOR('',#33337,10.);
#10260=VECTOR('',#33338,10.);
#10261=VECTOR('',#33341,10.);
#10262=VECTOR('',#33342,10.);
#10263=VECTOR('',#33351,4.75);
#10264=VECTOR('',#33360,4.975);
#10265=VECTOR('',#33365,4.95);
#10266=VECTOR('',#33374,8.);
#10267=VECTOR('',#33375,8.);
#10268=VECTOR('',#33380,7.75);
#10269=VECTOR('',#33393,3.8);
#10270=VECTOR('',#33398,4.);
#10271=VECTOR('',#33403,3.8);
#10272=CIRCLE('',#25109,8.5);
#10273=CIRCLE('',#25110,9.);
#10274=CIRCLE('',#25112,5.55);
#10275=CIRCLE('',#25114,9.);
#10276=CIRCLE('',#25116,8.5);
#10277=CIRCLE('',#25117,9.);
#10278=CIRCLE('',#25119,5.55);
#10279=CIRCLE('',#25121,9.);
#10280=CIRCLE('',#25123,10.5);
#10281=CIRCLE('',#25124,10.);
#10282=CIRCLE('',#25125,10.);
#10283=CIRCLE('',#25127,10.);
#10284=CIRCLE('',#25129,14.3);
#10285=CIRCLE('',#25131,10.5);
#10286=CIRCLE('',#25133,20.95);
#10287=CIRCLE('',#25134,20.95);
#10288=CIRCLE('',#25137,26.5);
#10289=CIRCLE('',#25138,26.5);
#10290=CIRCLE('',#25139,26.5);
#10291=CIRCLE('',#25140,26.5);
#10292=CIRCLE('',#25141,45.5);
#10293=CIRCLE('',#25142,6.);
#10294=CIRCLE('',#25143,45.5);
#10295=CIRCLE('',#25144,45.5);
#10296=CIRCLE('',#25145,9.5);
#10297=CIRCLE('',#25146,23.5);
#10298=CIRCLE('',#25147,23.5);
#10299=CIRCLE('',#25148,9.5);
#10300=CIRCLE('',#25149,45.5);
#10301=CIRCLE('',#25150,45.5);
#10302=CIRCLE('',#25151,23.5);
#10303=CIRCLE('',#25152,9.5);
#10304=CIRCLE('',#25153,45.5);
#10305=CIRCLE('',#25154,6.55);
#10306=CIRCLE('',#25155,41.28);
#10307=CIRCLE('',#25156,41.28);
#10308=CIRCLE('',#25157,6.55);
#10309=CIRCLE('',#25158,41.28);
#10310=CIRCLE('',#25159,23.5);
#10311=CIRCLE('',#25160,45.5);
#10312=CIRCLE('',#25161,9.5);
#10313=CIRCLE('',#25162,6.);
#10314=CIRCLE('',#25169,5.05);
#10315=CIRCLE('',#25171,5.05);
#10316=CIRCLE('',#25173,5.05);
#10317=CIRCLE('',#25175,5.05);
#10318=CIRCLE('',#25178,5.05);
#10319=CIRCLE('',#25179,5.05);
#10320=CIRCLE('',#25180,5.05);
#10321=CIRCLE('',#25181,5.05);
#10322=CIRCLE('',#25184,5.05);
#10323=CIRCLE('',#25185,5.05);
#10324=CIRCLE('',#25186,5.05);
#10325=CIRCLE('',#25187,5.05);
#10326=CIRCLE('',#25191,5.55);
#10327=CIRCLE('',#25193,26.5);
#10328=CIRCLE('',#25194,26.5);
#10329=CIRCLE('',#25195,26.5);
#10330=CIRCLE('',#25196,26.5);
#10331=CIRCLE('',#25197,5.55);
#10332=CIRCLE('',#25198,5.55);
#10333=CIRCLE('',#25199,6.);
#10334=CIRCLE('',#25200,26.05);
#10335=CIRCLE('',#25201,26.05);
#10336=CIRCLE('',#25202,4.01);
#10337=CIRCLE('',#25203,4.01);
#10338=CIRCLE('',#25204,6.);
#10339=CIRCLE('',#25205,5.55);
#10340=CIRCLE('',#25210,5.5);
#10341=CIRCLE('',#25212,5.5);
#10342=CIRCLE('',#25214,5.5);
#10343=CIRCLE('',#25216,5.5);
#10344=CIRCLE('',#25227,1.5);
#10345=CIRCLE('',#25228,0.999999999999995);
#10346=CIRCLE('',#25231,1.5);
#10347=CIRCLE('',#25232,0.999999999999996);
#10348=CIRCLE('',#25236,47.);
#10349=CIRCLE('',#25237,45.5);
#10350=CIRCLE('',#25239,47.);
#10351=CIRCLE('',#25241,11.);
#10352=CIRCLE('',#25243,47.);
#10353=CIRCLE('',#25245,1.5);
#10354=CIRCLE('',#25246,22.);
#10355=CIRCLE('',#25247,1.5);
#10356=CIRCLE('',#25251,47.);
#10357=CIRCLE('',#25254,22.);
#10358=CIRCLE('',#25256,47.);
#10359=CIRCLE('',#25258,11.);
#10360=CIRCLE('',#25260,1.5);
#10361=CIRCLE('',#25261,22.);
#10362=CIRCLE('',#25262,1.5);
#10363=CIRCLE('',#25266,11.);
#10364=CIRCLE('',#25269,22.);
#10365=CIRCLE('',#25272,47.);
#10366=CIRCLE('',#25274,47.);
#10367=CIRCLE('',#25276,11.);
#10368=CIRCLE('',#25278,11.);
#10369=CIRCLE('',#25280,1.5);
#10370=CIRCLE('',#25282,11.);
#10371=CIRCLE('',#25284,47.);
#10372=CIRCLE('',#25286,1.49999999999999);
#10373=CIRCLE('',#25287,22.);
#10374=CIRCLE('',#25289,1.5);
#10375=CIRCLE('',#25291,1.5);
#10376=CIRCLE('',#25292,22.);
#10377=CIRCLE('',#25296,22.);
#10378=CIRCLE('',#25299,22.);
#10379=CIRCLE('',#25302,11.);
#10380=CIRCLE('',#25304,47.);
#10381=CIRCLE('',#25306,1.5);
#10382=CIRCLE('',#25307,1.5);
#10383=CIRCLE('',#25309,1.49999999999999);
#10384=CIRCLE('',#25310,28.);
#10385=CIRCLE('',#25312,1.5);
#10386=CIRCLE('',#25314,1.5);
#10387=CIRCLE('',#25315,28.);
#10388=CIRCLE('',#25317,1.5);
#10389=CIRCLE('',#25319,1.5);
#10390=CIRCLE('',#25320,28.);
#10391=CIRCLE('',#25323,1.5);
#10392=CIRCLE('',#25324,28.);
#10393=CIRCLE('',#25327,28.);
#10394=CIRCLE('',#25330,28.);
#10395=CIRCLE('',#25333,28.);
#10396=CIRCLE('',#25339,47.);
#10397=CIRCLE('',#25342,47.);
#10398=CIRCLE('',#25344,47.);
#10399=CIRCLE('',#25347,47.);
#10400=CIRCLE('',#25349,1.5);
#10401=CIRCLE('',#25350,1.49999999999999);
#10402=CIRCLE('',#25352,1.5);
#10403=CIRCLE('',#25354,1.49999999999999);
#10404=CIRCLE('',#25356,1.5);
#10405=CIRCLE('',#25358,1.49999999999999);
#10406=CIRCLE('',#25360,1.5);
#10407=CIRCLE('',#25362,1.5);
#10408=CIRCLE('',#25363,28.);
#10409=CIRCLE('',#25366,41.28);
#10410=CIRCLE('',#25367,1.5);
#10411=CIRCLE('',#25368,39.78);
#10412=CIRCLE('',#25370,41.28);
#10413=CIRCLE('',#25371,41.28);
#10414=CIRCLE('',#25373,14.3);
#10415=CIRCLE('',#25378,39.78);
#10416=CIRCLE('',#25382,39.78);
#10417=CIRCLE('',#25385,1.5);
#10418=CIRCLE('',#25386,1.5);
#10419=CIRCLE('',#25388,1.5);
#10420=CIRCLE('',#25389,24.55);
#10421=CIRCLE('',#25391,1.5);
#10422=CIRCLE('',#25393,24.55);
#10423=CIRCLE('',#25395,24.55);
#10424=CIRCLE('',#25398,1.5);
#10425=CIRCLE('',#25399,1.5);
#10426=CIRCLE('',#25401,1.5);
#10427=CIRCLE('',#25402,22.45);
#10428=CIRCLE('',#25404,1.5);
#10429=CIRCLE('',#25406,22.45);
#10430=CIRCLE('',#25408,22.45);
#10431=CIRCLE('',#25411,22.45);
#10432=CIRCLE('',#25414,24.55);
#10433=CIRCLE('',#25418,4.01);
#10434=CIRCLE('',#25421,4.01);
#10435=CIRCLE('',#25424,14.7);
#10436=CIRCLE('',#25425,14.3);
#10437=CIRCLE('',#25427,14.7);
#10438=CIRCLE('',#25429,14.3);
#10439=CIRCLE('',#25434,47.);
#10440=CIRCLE('',#25436,11.);
#10441=CIRCLE('',#25447,14.05);
#10442=CIRCLE('',#25448,13.55);
#10443=CIRCLE('',#25450,13.55);
#10444=CIRCLE('',#25452,21.);
#10445=CIRCLE('',#25454,14.05);
#10446=CIRCLE('',#25455,13.55);
#10447=CIRCLE('',#25457,13.55);
#10448=CIRCLE('',#25459,21.);
#10449=CIRCLE('',#25461,0.800000000000001);
#10450=CIRCLE('',#25462,0.800000000000001);
#10451=CIRCLE('',#25464,0.799999999999992);
#10452=CIRCLE('',#25465,9.19999999999999);
#10453=CIRCLE('',#25466,9.99999999999999);
#10454=CIRCLE('',#25468,0.800000000000001);
#10455=CIRCLE('',#25470,0.800000000000005);
#10456=CIRCLE('',#25471,9.19999999999999);
#10457=CIRCLE('',#25472,9.99999999999999);
#10458=CIRCLE('',#25474,0.800000000000001);
#10459=CIRCLE('',#25476,0.800000000000001);
#10460=CIRCLE('',#25477,9.2);
#10461=CIRCLE('',#25478,9.99999999999999);
#10462=CIRCLE('',#25480,0.800000000000001);
#10463=CIRCLE('',#25482,9.19999999999999);
#10464=CIRCLE('',#25483,9.99999999999999);
#10465=CIRCLE('',#25485,9.99999999999999);
#10466=CIRCLE('',#25488,9.99999999999999);
#10467=CIRCLE('',#25490,21.);
#10468=CIRCLE('',#25492,4.01);
#10469=CIRCLE('',#25493,4.01);
#10470=CIRCLE('',#25494,19.3);
#10471=CIRCLE('',#25495,19.3);
#10472=CIRCLE('',#25496,5.3);
#10473=CIRCLE('',#25497,5.3);
#10474=CIRCLE('',#25498,5.3);
#10475=CIRCLE('',#25499,5.3);
#10476=CIRCLE('',#25501,0.800000000000001);
#10477=CIRCLE('',#25502,0.799999999999992);
#10478=CIRCLE('',#25504,0.800000000000001);
#10479=CIRCLE('',#25505,9.19999999999999);
#10480=CIRCLE('',#25506,9.99999999999999);
#10481=CIRCLE('',#25508,0.800000000000005);
#10482=CIRCLE('',#25510,0.799999999999996);
#10483=CIRCLE('',#25511,9.2);
#10484=CIRCLE('',#25512,9.99999999999999);
#10485=CIRCLE('',#25514,0.80000000000001);
#10486=CIRCLE('',#25516,0.800000000000001);
#10487=CIRCLE('',#25517,9.19999999999999);
#10488=CIRCLE('',#25519,0.799999999999992);
#10489=CIRCLE('',#25521,9.19999999999999);
#10490=CIRCLE('',#25526,4.01);
#10491=CIRCLE('',#25527,4.01);
#10492=CIRCLE('',#25528,19.3);
#10493=CIRCLE('',#25529,19.3);
#10494=CIRCLE('',#25530,5.3);
#10495=CIRCLE('',#25531,5.3);
#10496=CIRCLE('',#25532,5.3);
#10497=CIRCLE('',#25533,5.3);
#10498=CIRCLE('',#25535,4.01);
#10499=CIRCLE('',#25538,4.01);
#10500=CIRCLE('',#25541,4.01);
#10501=CIRCLE('',#25544,4.01);
#10502=CIRCLE('',#25551,8.);
#10503=CIRCLE('',#25555,21.);
#10504=CIRCLE('',#25557,8.);
#10505=CIRCLE('',#25564,7.2);
#10506=CIRCLE('',#25565,7.7);
#10507=CIRCLE('',#25567,11.);
#10508=CIRCLE('',#25569,7.2);
#10509=CIRCLE('',#25572,25.05);
#10510=CIRCLE('',#25573,24.55);
#10511=CIRCLE('',#25576,25.05);
#10512=CIRCLE('',#25577,24.55);
#10513=CIRCLE('',#25579,24.55);
#10514=CIRCLE('',#25582,9.49999999999999);
#10515=CIRCLE('',#25583,9.49999999999999);
#10516=CIRCLE('',#25584,9.49999999999999);
#10517=CIRCLE('',#25585,9.5);
#10518=CIRCLE('',#25586,5.3);
#10519=CIRCLE('',#25587,5.3);
#10520=CIRCLE('',#25588,5.3);
#10521=CIRCLE('',#25589,5.3);
#10522=CIRCLE('',#25590,4.01);
#10523=CIRCLE('',#25591,4.01);
#10524=CIRCLE('',#25594,21.95);
#10525=CIRCLE('',#25595,22.45);
#10526=CIRCLE('',#25598,21.95);
#10527=CIRCLE('',#25599,22.45);
#10528=CIRCLE('',#25601,22.45);
#10529=CIRCLE('',#25605,8.5);
#10530=CIRCLE('',#25606,9.);
#10531=CIRCLE('',#25609,8.5);
#10532=CIRCLE('',#25611,8.5);
#10533=CIRCLE('',#25612,9.);
#10534=CIRCLE('',#25614,8.5);
#10535=CIRCLE('',#25616,8.5);
#10536=CIRCLE('',#25617,8.5);
#10537=CIRCLE('',#25618,9.);
#10538=CIRCLE('',#25621,8.5);
#10539=CIRCLE('',#25623,8.5);
#10540=CIRCLE('',#25624,8.5);
#10541=CIRCLE('',#25625,9.);
#10542=CIRCLE('',#25627,8.5);
#10543=CIRCLE('',#25629,9.99999999999999);
#10544=CIRCLE('',#25632,10.);
#10545=CIRCLE('',#25635,9.99999999999999);
#10546=CIRCLE('',#25638,9.99999999999999);
#10547=CIRCLE('',#25642,9.99999999999999);
#10548=CIRCLE('',#25645,9.99999999999999);
#10549=CIRCLE('',#25648,9.64644660940673);
#10550=CIRCLE('',#25651,9.64644660940672);
#10551=CIRCLE('',#25654,9.64644660940673);
#10552=CIRCLE('',#25655,10.);
#10553=CIRCLE('',#25658,9.64644660940671);
#10554=CIRCLE('',#25659,9.99999999999999);
#10555=CIRCLE('',#25661,8.49999999999999);
#10556=CIRCLE('',#25664,8.49999999999999);
#10557=CIRCLE('',#25666,8.49999999999999);
#10558=CIRCLE('',#25669,8.49999999999999);
#10559=CIRCLE('',#25671,11.);
#10560=CIRCLE('',#25673,22.45);
#10561=CIRCLE('',#25676,24.55);
#10562=CIRCLE('',#25682,4.01);
#10563=CIRCLE('',#25685,4.01);
#10564=CIRCLE('',#25688,5.3);
#10565=CIRCLE('',#25690,5.3);
#10566=CIRCLE('',#25692,5.3);
#10567=CIRCLE('',#25694,5.3);
#10568=CIRCLE('',#25706,8.5);
#10569=CIRCLE('',#25780,8.5);
#10570=CIRCLE('',#25805,7.94);
#10571=CIRCLE('',#25809,7.94);
#10572=CIRCLE('',#26052,8.5);
#10573=CIRCLE('',#26054,7.44);
#10574=CIRCLE('',#26056,7.94);
#10575=CIRCLE('',#26058,7.94);
#10576=CIRCLE('',#26061,8.5);
#10577=CIRCLE('',#26066,8.5);
#10578=CIRCLE('',#26140,8.5);
#10579=CIRCLE('',#26405,8.5);
#10580=CIRCLE('',#26408,8.5);
#10581=CIRCLE('',#26422,11.5);
#10582=CIRCLE('',#26423,11.5);
#10583=CIRCLE('',#26425,11.5);
#10584=CIRCLE('',#26426,11.5);
#10585=CIRCLE('',#26428,19.25);
#10586=CIRCLE('',#26429,19.25);
#10587=CIRCLE('',#26431,19.25);
#10588=CIRCLE('',#26432,19.25);
#10589=CIRCLE('',#26437,9.69815599727615);
#10590=CIRCLE('',#26438,9.69815599727615);
#10591=CIRCLE('',#26439,9.25);
#10592=CIRCLE('',#26441,7.94);
#10593=CIRCLE('',#26443,10.8);
#10594=CIRCLE('',#26445,7.94);
#10595=CIRCLE('',#26447,14.29);
#10596=CIRCLE('',#26449,14.29);
#10597=CIRCLE('',#26451,12.);
#10598=CIRCLE('',#26453,12.);
#10599=CIRCLE('',#26455,10.2);
#10600=CIRCLE('',#26461,12.2);
#10601=CIRCLE('',#26462,12.4);
#10602=CIRCLE('',#26467,12.2);
#10603=CIRCLE('',#26472,12.4);
#10604=CIRCLE('',#26476,14.7);
#10605=CIRCLE('',#26477,1.);
#10606=CIRCLE('',#26478,1.);
#10607=CIRCLE('',#26480,14.7);
#10608=CIRCLE('',#26482,0.800000000000001);
#10609=CIRCLE('',#26484,0.800000000000001);
#10610=CIRCLE('',#26486,1.);
#10611=CIRCLE('',#26488,1.);
#10612=CIRCLE('',#26490,0.800000000000001);
#10613=CIRCLE('',#26492,0.800000000000001);
#10614=CIRCLE('',#26515,1.);
#10615=CIRCLE('',#26516,1.);
#10616=CIRCLE('',#26517,22.5);
#10617=CIRCLE('',#26518,1.);
#10618=CIRCLE('',#26519,1.);
#10619=CIRCLE('',#26521,1.);
#10620=CIRCLE('',#26522,1.);
#10621=CIRCLE('',#26524,22.5);
#10622=CIRCLE('',#26525,1.);
#10623=CIRCLE('',#26526,1.);
#10624=CIRCLE('',#26551,6.2);
#10625=CIRCLE('',#26562,8.4732);
#10626=CIRCLE('',#26572,6.64);
#10627=CIRCLE('',#26574,7.14);
#10628=CIRCLE('',#26576,7.14);
#10629=CIRCLE('',#26578,6.2);
#10630=CIRCLE('',#26582,8.5);
#10631=CIRCLE('',#26583,8.5);
#10632=CIRCLE('',#26585,10.7);
#10633=CIRCLE('',#26587,10.7);
#10634=CIRCLE('',#26589,10.7);
#10635=CIRCLE('',#26591,9.);
#10636=CIRCLE('',#26592,9.);
#10637=CIRCLE('',#26594,11.5);
#10638=CIRCLE('',#26596,11.5);
#10639=CIRCLE('',#26598,9.);
#10640=CIRCLE('',#26600,9.);
#10641=CIRCLE('',#26603,10.7);
#10642=CIRCLE('',#26607,4.925);
#10643=CIRCLE('',#26628,4.925);
#10644=CIRCLE('',#26630,4.0705);
#10645=CIRCLE('',#26651,4.925);
#10646=CIRCLE('',#26653,4.925);
#10647=CIRCLE('',#26654,4.925);
#10648=CIRCLE('',#26655,4.0705);
#10649=CIRCLE('',#26659,8.);
#10650=CIRCLE('',#26662,8.);
#10651=CIRCLE('',#26665,8.);
#10652=CIRCLE('',#26668,8.);
#10653=CIRCLE('',#26671,8.);
#10654=CIRCLE('',#26674,8.);
#10655=CIRCLE('',#26677,8.);
#10656=CIRCLE('',#26680,8.);
#10657=CIRCLE('',#26683,8.);
#10658=CIRCLE('',#26686,8.);
#10659=CIRCLE('',#26689,8.);
#10660=CIRCLE('',#26692,8.);
#10661=CIRCLE('',#26695,8.);
#10662=CIRCLE('',#26698,8.);
#10663=CIRCLE('',#26701,8.);
#10664=CIRCLE('',#26704,8.);
#10665=CIRCLE('',#26707,8.);
#10666=CIRCLE('',#26710,8.);
#10667=CIRCLE('',#26713,8.);
#10668=CIRCLE('',#26716,8.);
#10669=CIRCLE('',#26719,8.);
#10670=CIRCLE('',#26722,8.);
#10671=CIRCLE('',#26725,8.);
#10672=CIRCLE('',#26728,8.);
#10673=CIRCLE('',#26731,8.);
#10674=CIRCLE('',#26734,8.);
#10675=CIRCLE('',#26737,8.);
#10676=CIRCLE('',#26740,8.);
#10677=CIRCLE('',#26743,8.);
#10678=CIRCLE('',#26746,8.);
#10679=CIRCLE('',#26749,8.);
#10680=CIRCLE('',#26752,8.);
#10681=CIRCLE('',#26755,8.);
#10682=CIRCLE('',#26758,8.);
#10683=CIRCLE('',#26761,8.);
#10684=CIRCLE('',#26762,8.);
#10685=CIRCLE('',#26765,8.);
#10686=CIRCLE('',#26766,8.);
#10687=CIRCLE('',#26769,8.);
#10688=CIRCLE('',#26772,8.);
#10689=CIRCLE('',#26775,8.);
#10690=CIRCLE('',#26778,8.);
#10691=CIRCLE('',#26781,8.);
#10692=CIRCLE('',#26784,8.);
#10693=CIRCLE('',#26787,8.);
#10694=CIRCLE('',#26790,8.);
#10695=CIRCLE('',#26793,8.);
#10696=CIRCLE('',#26796,8.);
#10697=CIRCLE('',#26799,8.);
#10698=CIRCLE('',#26802,8.);
#10699=CIRCLE('',#26805,8.);
#10700=CIRCLE('',#26808,8.);
#10701=CIRCLE('',#26811,8.);
#10702=CIRCLE('',#26814,8.);
#10703=CIRCLE('',#26817,8.);
#10704=CIRCLE('',#26820,8.);
#10705=CIRCLE('',#26823,8.);
#10706=CIRCLE('',#26826,8.);
#10707=CIRCLE('',#26829,8.);
#10708=CIRCLE('',#26832,8.);
#10709=CIRCLE('',#26835,8.);
#10710=CIRCLE('',#26838,8.);
#10711=CIRCLE('',#26841,8.);
#10712=CIRCLE('',#26844,8.);
#10713=CIRCLE('',#26847,8.);
#10714=CIRCLE('',#26850,8.);
#10715=CIRCLE('',#26853,8.);
#10716=CIRCLE('',#26856,8.);
#10717=CIRCLE('',#26859,8.);
#10718=CIRCLE('',#26862,8.);
#10719=CIRCLE('',#26865,8.);
#10720=CIRCLE('',#26868,8.);
#10721=CIRCLE('',#26871,8.);
#10722=CIRCLE('',#26874,8.);
#10723=CIRCLE('',#26883,4.5);
#10724=CIRCLE('',#26886,4.925);
#10725=CIRCLE('',#26888,4.95);
#10726=CIRCLE('',#26890,4.95);
#10727=CIRCLE('',#26892,8.);
#10728=CIRCLE('',#26894,8.);
#10729=CIRCLE('',#26896,7.5);
#10730=CIRCLE('',#26900,3.6);
#10731=CIRCLE('',#26902,4.);
#10732=CIRCLE('',#26904,4.);
#10733=CIRCLE('',#26906,3.6);
#10734=VERTEX_POINT('',#33459);
#10735=VERTEX_POINT('',#33461);
#10736=VERTEX_POINT('',#33465);
#10737=VERTEX_POINT('',#33468);
#10738=VERTEX_POINT('',#33472);
#10739=VERTEX_POINT('',#33474);
#10740=VERTEX_POINT('',#33478);
#10741=VERTEX_POINT('',#33481);
#10742=VERTEX_POINT('',#33485);
#10743=VERTEX_POINT('',#33487);
#10744=VERTEX_POINT('',#33489);
#10745=VERTEX_POINT('',#33493);
#10746=VERTEX_POINT('',#33497);
#10747=VERTEX_POINT('',#33500);
#10748=VERTEX_POINT('',#33504);
#10749=VERTEX_POINT('',#33505);
#10750=VERTEX_POINT('',#33507);
#10751=VERTEX_POINT('',#33509);
#10752=VERTEX_POINT('',#33536);
#10753=VERTEX_POINT('',#33537);
#10754=VERTEX_POINT('',#33593);
#10755=VERTEX_POINT('',#33598);
#10756=VERTEX_POINT('',#33679);
#10757=VERTEX_POINT('',#33686);
#10758=VERTEX_POINT('',#33695);
#10759=VERTEX_POINT('',#33696);
#10760=VERTEX_POINT('',#33701);
#10761=VERTEX_POINT('',#33702);
#10762=VERTEX_POINT('',#33704);
#10763=VERTEX_POINT('',#33706);
#10764=VERTEX_POINT('',#33708);
#10765=VERTEX_POINT('',#33710);
#10766=VERTEX_POINT('',#33712);
#10767=VERTEX_POINT('',#33714);
#10768=VERTEX_POINT('',#33716);
#10769=VERTEX_POINT('',#33718);
#10770=VERTEX_POINT('',#33721);
#10771=VERTEX_POINT('',#33723);
#10772=VERTEX_POINT('',#33725);
#10773=VERTEX_POINT('',#33727);
#10774=VERTEX_POINT('',#33729);
#10775=VERTEX_POINT('',#33731);
#10776=VERTEX_POINT('',#33733);
#10777=VERTEX_POINT('',#33735);
#10778=VERTEX_POINT('',#33737);
#10779=VERTEX_POINT('',#33739);
#10780=VERTEX_POINT('',#33741);
#10781=VERTEX_POINT('',#33743);
#10782=VERTEX_POINT('',#33745);
#10783=VERTEX_POINT('',#33747);
#10784=VERTEX_POINT('',#33749);
#10785=VERTEX_POINT('',#33751);
#10786=VERTEX_POINT('',#33753);
#10787=VERTEX_POINT('',#33755);
#10788=VERTEX_POINT('',#33757);
#10789=VERTEX_POINT('',#33759);
#10790=VERTEX_POINT('',#33761);
#10791=VERTEX_POINT('',#33763);
#10792=VERTEX_POINT('',#33765);
#10793=VERTEX_POINT('',#33768);
#10794=VERTEX_POINT('',#33769);
#10795=VERTEX_POINT('',#33771);
#10796=VERTEX_POINT('',#33773);
#10797=VERTEX_POINT('',#33775);
#10798=VERTEX_POINT('',#33778);
#10799=VERTEX_POINT('',#33779);
#10800=VERTEX_POINT('',#33781);
#10801=VERTEX_POINT('',#33783);
#10802=VERTEX_POINT('',#33785);
#10803=VERTEX_POINT('',#33788);
#10804=VERTEX_POINT('',#33789);
#10805=VERTEX_POINT('',#33791);
#10806=VERTEX_POINT('',#33793);
#10807=VERTEX_POINT('',#33795);
#10808=VERTEX_POINT('',#33798);
#10809=VERTEX_POINT('',#33801);
#10810=VERTEX_POINT('',#33803);
#10811=VERTEX_POINT('',#33867);
#10812=VERTEX_POINT('',#33894);
#10813=VERTEX_POINT('',#33982);
#10814=VERTEX_POINT('',#33992);
#10815=VERTEX_POINT('',#33996);
#10816=VERTEX_POINT('',#34013);
#10817=VERTEX_POINT('',#34017);
#10818=VERTEX_POINT('',#34021);
#10819=VERTEX_POINT('',#34025);
#10820=VERTEX_POINT('',#34029);
#10821=VERTEX_POINT('',#34033);
#10822=VERTEX_POINT('',#34034);
#10823=VERTEX_POINT('',#34041);
#10824=VERTEX_POINT('',#34043);
#10825=VERTEX_POINT('',#34052);
#10826=VERTEX_POINT('',#34054);
#10827=VERTEX_POINT('',#34056);
#10828=VERTEX_POINT('',#34066);
#10829=VERTEX_POINT('',#34068);
#10830=VERTEX_POINT('',#34070);
#10831=VERTEX_POINT('',#34081);
#10832=VERTEX_POINT('',#34082);
#10833=VERTEX_POINT('',#34089);
#10834=VERTEX_POINT('',#34091);
#10835=VERTEX_POINT('',#34100);
#10836=VERTEX_POINT('',#34102);
#10837=VERTEX_POINT('',#34105);
#10838=VERTEX_POINT('',#34114);
#10839=VERTEX_POINT('',#34116);
#10840=VERTEX_POINT('',#34125);
#10841=VERTEX_POINT('',#34129);
#10842=VERTEX_POINT('',#34136);
#10843=VERTEX_POINT('',#34145);
#10844=VERTEX_POINT('',#34152);
#10845=VERTEX_POINT('',#34161);
#10846=VERTEX_POINT('',#34165);
#10847=VERTEX_POINT('',#34166);
#10848=VERTEX_POINT('',#34168);
#10849=VERTEX_POINT('',#34170);
#10850=VERTEX_POINT('',#34172);
#10851=VERTEX_POINT('',#34174);
#10852=VERTEX_POINT('',#34176);
#10853=VERTEX_POINT('',#34178);
#10854=VERTEX_POINT('',#34181);
#10855=VERTEX_POINT('',#34183);
#10856=VERTEX_POINT('',#34185);
#10857=VERTEX_POINT('',#34187);
#10858=VERTEX_POINT('',#34188);
#10859=VERTEX_POINT('',#34190);
#10860=VERTEX_POINT('',#34192);
#10861=VERTEX_POINT('',#34195);
#10862=VERTEX_POINT('',#34197);
#10863=VERTEX_POINT('',#34199);
#10864=VERTEX_POINT('',#34201);
#10865=VERTEX_POINT('',#34210);
#10866=VERTEX_POINT('',#34214);
#10867=VERTEX_POINT('',#34218);
#10868=VERTEX_POINT('',#34222);
#10869=VERTEX_POINT('',#34249);
#10870=VERTEX_POINT('',#34305);
#10871=VERTEX_POINT('',#34389);
#10872=VERTEX_POINT('',#34396);
#10873=VERTEX_POINT('',#34405);
#10874=VERTEX_POINT('',#34406);
#10875=VERTEX_POINT('',#34411);
#10876=VERTEX_POINT('',#34413);
#10877=VERTEX_POINT('',#34476);
#10878=VERTEX_POINT('',#34503);
#10879=VERTEX_POINT('',#34587);
#10880=VERTEX_POINT('',#34596);
#10881=VERTEX_POINT('',#34600);
#10882=VERTEX_POINT('',#34617);
#10883=VERTEX_POINT('',#34625);
#10884=VERTEX_POINT('',#34626);
#10885=VERTEX_POINT('',#34628);
#10886=VERTEX_POINT('',#34630);
#10887=VERTEX_POINT('',#34634);
#10888=VERTEX_POINT('',#34639);
#10889=VERTEX_POINT('',#34643);
#10890=VERTEX_POINT('',#34644);
#10891=VERTEX_POINT('',#34649);
#10892=VERTEX_POINT('',#34650);
#10893=VERTEX_POINT('',#34657);
#10894=VERTEX_POINT('',#34658);
#10895=VERTEX_POINT('',#34671);
#10896=VERTEX_POINT('',#34673);
#10897=VERTEX_POINT('',#34688);
#10898=VERTEX_POINT('',#34690);
#10899=VERTEX_POINT('',#34694);
#10900=VERTEX_POINT('',#34709);
#10901=VERTEX_POINT('',#34726);
#10902=VERTEX_POINT('',#34743);
#10903=VERTEX_POINT('',#34745);
#10904=VERTEX_POINT('',#34753);
#10905=VERTEX_POINT('',#34755);
#10906=VERTEX_POINT('',#34759);
#10907=VERTEX_POINT('',#34763);
#10908=VERTEX_POINT('',#34767);
#10909=VERTEX_POINT('',#34782);
#10910=VERTEX_POINT('',#34799);
#10911=VERTEX_POINT('',#34816);
#10912=VERTEX_POINT('',#34818);
#10913=VERTEX_POINT('',#34826);
#10914=VERTEX_POINT('',#34828);
#10915=VERTEX_POINT('',#34832);
#10916=VERTEX_POINT('',#34836);
#10917=VERTEX_POINT('',#34869);
#10918=VERTEX_POINT('',#34886);
#10919=VERTEX_POINT('',#34890);
#10920=VERTEX_POINT('',#34905);
#10921=VERTEX_POINT('',#34922);
#10922=VERTEX_POINT('',#34924);
#10923=VERTEX_POINT('',#34928);
#10924=VERTEX_POINT('',#34929);
#10925=VERTEX_POINT('',#34947);
#10926=VERTEX_POINT('',#34964);
#10927=VERTEX_POINT('',#34981);
#10928=VERTEX_POINT('',#34985);
#10929=VERTEX_POINT('',#34989);
#10930=VERTEX_POINT('',#34995);
#10931=VERTEX_POINT('',#34999);
#10932=VERTEX_POINT('',#35003);
#10933=VERTEX_POINT('',#35007);
#10934=VERTEX_POINT('',#35011);
#10935=VERTEX_POINT('',#35015);
#10936=VERTEX_POINT('',#35019);
#10937=VERTEX_POINT('',#35023);
#10938=VERTEX_POINT('',#35025);
#10939=VERTEX_POINT('',#35029);
#10940=VERTEX_POINT('',#35033);
#10941=VERTEX_POINT('',#35037);
#10942=VERTEX_POINT('',#35041);
#10943=VERTEX_POINT('',#35045);
#10944=VERTEX_POINT('',#35051);
#10945=VERTEX_POINT('',#35057);
#10946=VERTEX_POINT('',#35059);
#10947=VERTEX_POINT('',#35063);
#10948=VERTEX_POINT('',#35067);
#10949=VERTEX_POINT('',#35071);
#10950=VERTEX_POINT('',#35075);
#10951=VERTEX_POINT('',#35087);
#10952=VERTEX_POINT('',#35104);
#10953=VERTEX_POINT('',#35123);
#10954=VERTEX_POINT('',#35127);
#10955=VERTEX_POINT('',#35144);
#10956=VERTEX_POINT('',#35148);
#10957=VERTEX_POINT('',#35154);
#10958=VERTEX_POINT('',#35156);
#10959=VERTEX_POINT('',#35192);
#10960=VERTEX_POINT('',#35207);
#10961=VERTEX_POINT('',#35209);
#10962=VERTEX_POINT('',#35213);
#10963=VERTEX_POINT('',#35217);
#10964=VERTEX_POINT('',#35223);
#10965=VERTEX_POINT('',#35225);
#10966=VERTEX_POINT('',#35229);
#10967=VERTEX_POINT('',#35233);
#10968=VERTEX_POINT('',#35235);
#10969=VERTEX_POINT('',#35239);
#10970=VERTEX_POINT('',#35243);
#10971=VERTEX_POINT('',#35249);
#10972=VERTEX_POINT('',#35251);
#10973=VERTEX_POINT('',#35255);
#10974=VERTEX_POINT('',#35259);
#10975=VERTEX_POINT('',#35265);
#10976=VERTEX_POINT('',#35272);
#10977=VERTEX_POINT('',#35277);
#10978=VERTEX_POINT('',#35282);
#10979=VERTEX_POINT('',#35284);
#10980=VERTEX_POINT('',#35287);
#10981=VERTEX_POINT('',#35291);
#10982=VERTEX_POINT('',#35299);
#10983=VERTEX_POINT('',#35303);
#10984=VERTEX_POINT('',#35321);
#10985=VERTEX_POINT('',#35323);
#10986=VERTEX_POINT('',#35327);
#10987=VERTEX_POINT('',#35331);
#10988=VERTEX_POINT('',#35334);
#10989=VERTEX_POINT('',#35336);
#10990=VERTEX_POINT('',#35340);
#10991=VERTEX_POINT('',#35344);
#10992=VERTEX_POINT('',#35347);
#10993=VERTEX_POINT('',#35348);
#10994=VERTEX_POINT('',#35350);
#10995=VERTEX_POINT('',#35352);
#10996=VERTEX_POINT('',#35356);
#10997=VERTEX_POINT('',#35357);
#10998=VERTEX_POINT('',#35362);
#10999=VERTEX_POINT('',#35363);
#11000=VERTEX_POINT('',#35368);
#11001=VERTEX_POINT('',#35369);
#11002=VERTEX_POINT('',#35374);
#11003=VERTEX_POINT('',#35375);
#11004=VERTEX_POINT('',#35380);
#11005=VERTEX_POINT('',#35381);
#11006=VERTEX_POINT('',#35386);
#11007=VERTEX_POINT('',#35387);
#11008=VERTEX_POINT('',#35395);
#11009=VERTEX_POINT('',#35397);
#11010=VERTEX_POINT('',#35401);
#11011=VERTEX_POINT('',#35405);
#11012=VERTEX_POINT('',#35409);
#11013=VERTEX_POINT('',#35412);
#11014=VERTEX_POINT('',#35415);
#11015=VERTEX_POINT('',#35417);
#11016=VERTEX_POINT('',#35419);
#11017=VERTEX_POINT('',#35420);
#11018=VERTEX_POINT('',#35423);
#11019=VERTEX_POINT('',#35425);
#11020=VERTEX_POINT('',#35427);
#11021=VERTEX_POINT('',#35429);
#11022=VERTEX_POINT('',#35432);
#11023=VERTEX_POINT('',#35434);
#11024=VERTEX_POINT('',#35438);
#11025=VERTEX_POINT('',#35439);
#11026=VERTEX_POINT('',#35444);
#11027=VERTEX_POINT('',#35445);
#11028=VERTEX_POINT('',#35450);
#11029=VERTEX_POINT('',#35451);
#11030=VERTEX_POINT('',#35456);
#11031=VERTEX_POINT('',#35461);
#11032=VERTEX_POINT('',#35465);
#11033=VERTEX_POINT('',#35477);
#11034=VERTEX_POINT('',#35479);
#11035=VERTEX_POINT('',#35481);
#11036=VERTEX_POINT('',#35482);
#11037=VERTEX_POINT('',#35485);
#11038=VERTEX_POINT('',#35487);
#11039=VERTEX_POINT('',#35489);
#11040=VERTEX_POINT('',#35491);
#11041=VERTEX_POINT('',#35494);
#11042=VERTEX_POINT('',#35499);
#11043=VERTEX_POINT('',#35504);
#11044=VERTEX_POINT('',#35509);
#11045=VERTEX_POINT('',#35522);
#11046=VERTEX_POINT('',#35524);
#11047=VERTEX_POINT('',#35526);
#11048=VERTEX_POINT('',#35541);
#11049=VERTEX_POINT('',#35584);
#11050=VERTEX_POINT('',#35586);
#11051=VERTEX_POINT('',#35601);
#11052=VERTEX_POINT('',#35620);
#11053=VERTEX_POINT('',#35624);
#11054=VERTEX_POINT('',#35660);
#11055=VERTEX_POINT('',#35662);
#11056=VERTEX_POINT('',#35666);
#11057=VERTEX_POINT('',#35669);
#11058=VERTEX_POINT('',#35673);
#11059=VERTEX_POINT('',#35674);
#11060=VERTEX_POINT('',#35676);
#11061=VERTEX_POINT('',#35678);
#11062=VERTEX_POINT('',#35682);
#11063=VERTEX_POINT('',#35683);
#11064=VERTEX_POINT('',#35688);
#11065=VERTEX_POINT('',#35689);
#11066=VERTEX_POINT('',#35697);
#11067=VERTEX_POINT('',#35699);
#11068=VERTEX_POINT('',#35703);
#11069=VERTEX_POINT('',#35707);
#11070=VERTEX_POINT('',#35708);
#11071=VERTEX_POINT('',#35710);
#11072=VERTEX_POINT('',#35712);
#11073=VERTEX_POINT('',#35714);
#11074=VERTEX_POINT('',#35716);
#11075=VERTEX_POINT('',#35718);
#11076=VERTEX_POINT('',#35720);
#11077=VERTEX_POINT('',#35723);
#11078=VERTEX_POINT('',#35725);
#11079=VERTEX_POINT('',#35727);
#11080=VERTEX_POINT('',#35729);
#11081=VERTEX_POINT('',#35731);
#11082=VERTEX_POINT('',#35733);
#11083=VERTEX_POINT('',#35736);
#11084=VERTEX_POINT('',#35737);
#11085=VERTEX_POINT('',#35739);
#11086=VERTEX_POINT('',#35741);
#11087=VERTEX_POINT('',#35745);
#11088=VERTEX_POINT('',#35746);
#11089=VERTEX_POINT('',#35751);
#11090=VERTEX_POINT('',#35752);
#11091=VERTEX_POINT('',#35760);
#11092=VERTEX_POINT('',#35762);
#11093=VERTEX_POINT('',#35766);
#11094=VERTEX_POINT('',#35771);
#11095=VERTEX_POINT('',#35772);
#11096=VERTEX_POINT('',#35776);
#11097=VERTEX_POINT('',#35779);
#11098=VERTEX_POINT('',#35785);
#11099=VERTEX_POINT('',#35787);
#11100=VERTEX_POINT('',#35791);
#11101=VERTEX_POINT('',#35795);
#11102=VERTEX_POINT('',#35797);
#11103=VERTEX_POINT('',#35799);
#11104=VERTEX_POINT('',#35801);
#11105=VERTEX_POINT('',#35805);
#11106=VERTEX_POINT('',#35809);
#11107=VERTEX_POINT('',#35814);
#11108=VERTEX_POINT('',#35818);
#11109=VERTEX_POINT('',#35819);
#11110=VERTEX_POINT('',#35823);
#11111=VERTEX_POINT('',#35825);
#11112=VERTEX_POINT('',#35828);
#11113=VERTEX_POINT('',#35834);
#11114=VERTEX_POINT('',#35836);
#11115=VERTEX_POINT('',#35840);
#11116=VERTEX_POINT('',#35844);
#11117=VERTEX_POINT('',#35846);
#11118=VERTEX_POINT('',#35848);
#11119=VERTEX_POINT('',#35850);
#11120=VERTEX_POINT('',#35854);
#11121=VERTEX_POINT('',#35858);
#11122=VERTEX_POINT('',#35860);
#11123=VERTEX_POINT('',#35865);
#11124=VERTEX_POINT('',#35869);
#11125=VERTEX_POINT('',#35871);
#11126=VERTEX_POINT('',#35875);
#11127=VERTEX_POINT('',#35879);
#11128=VERTEX_POINT('',#35883);
#11129=VERTEX_POINT('',#35887);
#11130=VERTEX_POINT('',#35891);
#11131=VERTEX_POINT('',#35895);
#11132=VERTEX_POINT('',#35901);
#11133=VERTEX_POINT('',#35903);
#11134=VERTEX_POINT('',#35907);
#11135=VERTEX_POINT('',#35911);
#11136=VERTEX_POINT('',#35915);
#11137=VERTEX_POINT('',#35922);
#11138=VERTEX_POINT('',#35926);
#11139=VERTEX_POINT('',#35933);
#11140=VERTEX_POINT('',#35937);
#11141=VERTEX_POINT('',#35938);
#11142=VERTEX_POINT('',#35943);
#11143=VERTEX_POINT('',#35944);
#11144=VERTEX_POINT('',#35952);
#11145=VERTEX_POINT('',#35956);
#11146=VERTEX_POINT('',#35962);
#11147=VERTEX_POINT('',#35966);
#11148=VERTEX_POINT('',#35972);
#11149=VERTEX_POINT('',#35975);
#11150=VERTEX_POINT('',#35981);
#11151=VERTEX_POINT('',#35991);
#11152=VERTEX_POINT('',#35996);
#11153=VERTEX_POINT('',#36001);
#11154=VERTEX_POINT('',#36005);
#11155=VERTEX_POINT('',#36009);
#11156=VERTEX_POINT('',#36013);
#11157=VERTEX_POINT('',#36029);
#11158=VERTEX_POINT('',#36030);
#11159=VERTEX_POINT('',#36032);
#11160=VERTEX_POINT('',#36034);
#11161=VERTEX_POINT('',#36036);
#11162=VERTEX_POINT('',#36038);
#11163=VERTEX_POINT('',#36042);
#11164=VERTEX_POINT('',#36044);
#11165=VERTEX_POINT('',#36046);
#11166=VERTEX_POINT('',#36048);
#11167=VERTEX_POINT('',#36050);
#11168=VERTEX_POINT('',#36052);
#11169=VERTEX_POINT('',#36054);
#11170=VERTEX_POINT('',#36056);
#11171=VERTEX_POINT('',#36058);
#11172=VERTEX_POINT('',#36060);
#11173=VERTEX_POINT('',#36062);
#11174=VERTEX_POINT('',#36064);
#11175=VERTEX_POINT('',#36066);
#11176=VERTEX_POINT('',#36068);
#11177=VERTEX_POINT('',#36070);
#11178=VERTEX_POINT('',#36072);
#11179=VERTEX_POINT('',#36074);
#11180=VERTEX_POINT('',#36076);
#11181=VERTEX_POINT('',#36078);
#11182=VERTEX_POINT('',#36080);
#11183=VERTEX_POINT('',#36082);
#11184=VERTEX_POINT('',#36084);
#11185=VERTEX_POINT('',#36086);
#11186=VERTEX_POINT('',#36088);
#11187=VERTEX_POINT('',#36090);
#11188=VERTEX_POINT('',#36092);
#11189=VERTEX_POINT('',#36094);
#11190=VERTEX_POINT('',#36096);
#11191=VERTEX_POINT('',#36098);
#11192=VERTEX_POINT('',#36100);
#11193=VERTEX_POINT('',#36102);
#11194=VERTEX_POINT('',#36104);
#11195=VERTEX_POINT('',#36106);
#11196=VERTEX_POINT('',#36108);
#11197=VERTEX_POINT('',#36110);
#11198=VERTEX_POINT('',#36112);
#11199=VERTEX_POINT('',#36114);
#11200=VERTEX_POINT('',#36116);
#11201=VERTEX_POINT('',#36118);
#11202=VERTEX_POINT('',#36120);
#11203=VERTEX_POINT('',#36122);
#11204=VERTEX_POINT('',#36124);
#11205=VERTEX_POINT('',#36126);
#11206=VERTEX_POINT('',#36128);
#11207=VERTEX_POINT('',#36130);
#11208=VERTEX_POINT('',#36132);
#11209=VERTEX_POINT('',#36134);
#11210=VERTEX_POINT('',#36136);
#11211=VERTEX_POINT('',#36138);
#11212=VERTEX_POINT('',#36140);
#11213=VERTEX_POINT('',#36142);
#11214=VERTEX_POINT('',#36144);
#11215=VERTEX_POINT('',#36146);
#11216=VERTEX_POINT('',#36148);
#11217=VERTEX_POINT('',#36150);
#11218=VERTEX_POINT('',#36152);
#11219=VERTEX_POINT('',#36154);
#11220=VERTEX_POINT('',#36156);
#11221=VERTEX_POINT('',#36158);
#11222=VERTEX_POINT('',#36160);
#11223=VERTEX_POINT('',#36162);
#11224=VERTEX_POINT('',#36164);
#11225=VERTEX_POINT('',#36166);
#11226=VERTEX_POINT('',#36168);
#11227=VERTEX_POINT('',#36170);
#11228=VERTEX_POINT('',#36172);
#11229=VERTEX_POINT('',#36174);
#11230=VERTEX_POINT('',#36176);
#11231=VERTEX_POINT('',#36178);
#11232=VERTEX_POINT('',#36180);
#11233=VERTEX_POINT('',#36182);
#11234=VERTEX_POINT('',#36184);
#11235=VERTEX_POINT('',#36186);
#11236=VERTEX_POINT('',#36188);
#11237=VERTEX_POINT('',#36190);
#11238=VERTEX_POINT('',#36192);
#11239=VERTEX_POINT('',#36194);
#11240=VERTEX_POINT('',#36196);
#11241=VERTEX_POINT('',#36198);
#11242=VERTEX_POINT('',#36200);
#11243=VERTEX_POINT('',#36202);
#11244=VERTEX_POINT('',#36204);
#11245=VERTEX_POINT('',#36206);
#11246=VERTEX_POINT('',#36208);
#11247=VERTEX_POINT('',#36210);
#11248=VERTEX_POINT('',#36212);
#11249=VERTEX_POINT('',#36214);
#11250=VERTEX_POINT('',#36216);
#11251=VERTEX_POINT('',#36218);
#11252=VERTEX_POINT('',#36220);
#11253=VERTEX_POINT('',#36222);
#11254=VERTEX_POINT('',#36224);
#11255=VERTEX_POINT('',#36226);
#11256=VERTEX_POINT('',#36228);
#11257=VERTEX_POINT('',#36230);
#11258=VERTEX_POINT('',#36232);
#11259=VERTEX_POINT('',#36234);
#11260=VERTEX_POINT('',#36236);
#11261=VERTEX_POINT('',#36238);
#11262=VERTEX_POINT('',#36240);
#11263=VERTEX_POINT('',#36242);
#11264=VERTEX_POINT('',#36244);
#11265=VERTEX_POINT('',#36246);
#11266=VERTEX_POINT('',#36248);
#11267=VERTEX_POINT('',#36250);
#11268=VERTEX_POINT('',#36252);
#11269=VERTEX_POINT('',#36254);
#11270=VERTEX_POINT('',#36256);
#11271=VERTEX_POINT('',#36258);
#11272=VERTEX_POINT('',#36260);
#11273=VERTEX_POINT('',#36262);
#11274=VERTEX_POINT('',#36264);
#11275=VERTEX_POINT('',#36266);
#11276=VERTEX_POINT('',#36268);
#11277=VERTEX_POINT('',#36270);
#11278=VERTEX_POINT('',#36272);
#11279=VERTEX_POINT('',#36274);
#11280=VERTEX_POINT('',#36276);
#11281=VERTEX_POINT('',#36278);
#11282=VERTEX_POINT('',#36280);
#11283=VERTEX_POINT('',#36282);
#11284=VERTEX_POINT('',#36284);
#11285=VERTEX_POINT('',#36286);
#11286=VERTEX_POINT('',#36288);
#11287=VERTEX_POINT('',#36290);
#11288=VERTEX_POINT('',#36292);
#11289=VERTEX_POINT('',#36294);
#11290=VERTEX_POINT('',#36296);
#11291=VERTEX_POINT('',#36298);
#11292=VERTEX_POINT('',#36300);
#11293=VERTEX_POINT('',#36302);
#11294=VERTEX_POINT('',#36304);
#11295=VERTEX_POINT('',#36306);
#11296=VERTEX_POINT('',#36308);
#11297=VERTEX_POINT('',#36310);
#11298=VERTEX_POINT('',#36312);
#11299=VERTEX_POINT('',#36314);
#11300=VERTEX_POINT('',#36316);
#11301=VERTEX_POINT('',#36318);
#11302=VERTEX_POINT('',#36320);
#11303=VERTEX_POINT('',#36322);
#11304=VERTEX_POINT('',#36324);
#11305=VERTEX_POINT('',#36326);
#11306=VERTEX_POINT('',#36328);
#11307=VERTEX_POINT('',#36330);
#11308=VERTEX_POINT('',#36332);
#11309=VERTEX_POINT('',#36334);
#11310=VERTEX_POINT('',#36336);
#11311=VERTEX_POINT('',#36338);
#11312=VERTEX_POINT('',#36340);
#11313=VERTEX_POINT('',#36342);
#11314=VERTEX_POINT('',#36344);
#11315=VERTEX_POINT('',#36346);
#11316=VERTEX_POINT('',#36348);
#11317=VERTEX_POINT('',#36350);
#11318=VERTEX_POINT('',#36352);
#11319=VERTEX_POINT('',#36354);
#11320=VERTEX_POINT('',#36356);
#11321=VERTEX_POINT('',#36358);
#11322=VERTEX_POINT('',#36360);
#11323=VERTEX_POINT('',#36362);
#11324=VERTEX_POINT('',#36364);
#11325=VERTEX_POINT('',#36366);
#11326=VERTEX_POINT('',#36368);
#11327=VERTEX_POINT('',#36370);
#11328=VERTEX_POINT('',#36372);
#11329=VERTEX_POINT('',#36374);
#11330=VERTEX_POINT('',#36376);
#11331=VERTEX_POINT('',#36378);
#11332=VERTEX_POINT('',#36380);
#11333=VERTEX_POINT('',#36382);
#11334=VERTEX_POINT('',#36384);
#11335=VERTEX_POINT('',#36386);
#11336=VERTEX_POINT('',#36388);
#11337=VERTEX_POINT('',#36390);
#11338=VERTEX_POINT('',#36392);
#11339=VERTEX_POINT('',#36394);
#11340=VERTEX_POINT('',#36396);
#11341=VERTEX_POINT('',#36398);
#11342=VERTEX_POINT('',#36400);
#11343=VERTEX_POINT('',#36402);
#11344=VERTEX_POINT('',#36404);
#11345=VERTEX_POINT('',#36406);
#11346=VERTEX_POINT('',#36408);
#11347=VERTEX_POINT('',#36410);
#11348=VERTEX_POINT('',#36412);
#11349=VERTEX_POINT('',#36414);
#11350=VERTEX_POINT('',#36416);
#11351=VERTEX_POINT('',#36418);
#11352=VERTEX_POINT('',#36420);
#11353=VERTEX_POINT('',#36422);
#11354=VERTEX_POINT('',#36424);
#11355=VERTEX_POINT('',#36426);
#11356=VERTEX_POINT('',#36428);
#11357=VERTEX_POINT('',#36430);
#11358=VERTEX_POINT('',#36432);
#11359=VERTEX_POINT('',#36434);
#11360=VERTEX_POINT('',#36436);
#11361=VERTEX_POINT('',#36438);
#11362=VERTEX_POINT('',#36440);
#11363=VERTEX_POINT('',#36442);
#11364=VERTEX_POINT('',#36444);
#11365=VERTEX_POINT('',#36446);
#11366=VERTEX_POINT('',#36448);
#11367=VERTEX_POINT('',#36450);
#11368=VERTEX_POINT('',#36452);
#11369=VERTEX_POINT('',#36454);
#11370=VERTEX_POINT('',#36456);
#11371=VERTEX_POINT('',#36458);
#11372=VERTEX_POINT('',#36460);
#11373=VERTEX_POINT('',#36462);
#11374=VERTEX_POINT('',#36464);
#11375=VERTEX_POINT('',#36466);
#11376=VERTEX_POINT('',#36468);
#11377=VERTEX_POINT('',#36470);
#11378=VERTEX_POINT('',#36472);
#11379=VERTEX_POINT('',#36474);
#11380=VERTEX_POINT('',#36476);
#11381=VERTEX_POINT('',#36478);
#11382=VERTEX_POINT('',#36480);
#11383=VERTEX_POINT('',#36482);
#11384=VERTEX_POINT('',#36484);
#11385=VERTEX_POINT('',#36486);
#11386=VERTEX_POINT('',#36488);
#11387=VERTEX_POINT('',#36490);
#11388=VERTEX_POINT('',#36492);
#11389=VERTEX_POINT('',#36494);
#11390=VERTEX_POINT('',#36496);
#11391=VERTEX_POINT('',#36498);
#11392=VERTEX_POINT('',#36500);
#11393=VERTEX_POINT('',#36502);
#11394=VERTEX_POINT('',#36504);
#11395=VERTEX_POINT('',#36506);
#11396=VERTEX_POINT('',#36508);
#11397=VERTEX_POINT('',#36510);
#11398=VERTEX_POINT('',#36512);
#11399=VERTEX_POINT('',#36514);
#11400=VERTEX_POINT('',#36516);
#11401=VERTEX_POINT('',#36519);
#11402=VERTEX_POINT('',#36522);
#11403=VERTEX_POINT('',#36524);
#11404=VERTEX_POINT('',#36526);
#11405=VERTEX_POINT('',#36530);
#11406=VERTEX_POINT('',#36534);
#11407=VERTEX_POINT('',#36536);
#11408=VERTEX_POINT('',#36538);
#11409=VERTEX_POINT('',#36540);
#11410=VERTEX_POINT('',#36544);
#11411=VERTEX_POINT('',#36546);
#11412=VERTEX_POINT('',#36548);
#11413=VERTEX_POINT('',#36552);
#11414=VERTEX_POINT('',#36556);
#11415=VERTEX_POINT('',#36558);
#11416=VERTEX_POINT('',#36560);
#11417=VERTEX_POINT('',#36562);
#11418=VERTEX_POINT('',#36566);
#11419=VERTEX_POINT('',#36568);
#11420=VERTEX_POINT('',#36570);
#11421=VERTEX_POINT('',#36574);
#11422=VERTEX_POINT('',#36578);
#11423=VERTEX_POINT('',#36580);
#11424=VERTEX_POINT('',#36582);
#11425=VERTEX_POINT('',#36584);
#11426=VERTEX_POINT('',#36588);
#11427=VERTEX_POINT('',#36590);
#11428=VERTEX_POINT('',#36592);
#11429=VERTEX_POINT('',#36596);
#11430=VERTEX_POINT('',#36600);
#11431=VERTEX_POINT('',#36602);
#11432=VERTEX_POINT('',#36604);
#11433=VERTEX_POINT('',#36606);
#11434=VERTEX_POINT('',#36610);
#11435=VERTEX_POINT('',#36612);
#11436=VERTEX_POINT('',#36614);
#11437=VERTEX_POINT('',#36618);
#11438=VERTEX_POINT('',#36622);
#11439=VERTEX_POINT('',#36624);
#11440=VERTEX_POINT('',#36626);
#11441=VERTEX_POINT('',#36628);
#11442=VERTEX_POINT('',#36632);
#11443=VERTEX_POINT('',#36634);
#11444=VERTEX_POINT('',#36636);
#11445=VERTEX_POINT('',#36640);
#11446=VERTEX_POINT('',#36644);
#11447=VERTEX_POINT('',#36646);
#11448=VERTEX_POINT('',#36648);
#11449=VERTEX_POINT('',#36650);
#11450=VERTEX_POINT('',#36654);
#11451=VERTEX_POINT('',#36656);
#11452=VERTEX_POINT('',#36658);
#11453=VERTEX_POINT('',#36662);
#11454=VERTEX_POINT('',#36666);
#11455=VERTEX_POINT('',#36668);
#11456=VERTEX_POINT('',#36670);
#11457=VERTEX_POINT('',#36672);
#11458=VERTEX_POINT('',#36676);
#11459=VERTEX_POINT('',#36678);
#11460=VERTEX_POINT('',#36680);
#11461=VERTEX_POINT('',#36684);
#11462=VERTEX_POINT('',#36688);
#11463=VERTEX_POINT('',#36690);
#11464=VERTEX_POINT('',#36692);
#11465=VERTEX_POINT('',#36694);
#11466=VERTEX_POINT('',#36698);
#11467=VERTEX_POINT('',#36700);
#11468=VERTEX_POINT('',#36702);
#11469=VERTEX_POINT('',#36706);
#11470=VERTEX_POINT('',#36710);
#11471=VERTEX_POINT('',#36712);
#11472=VERTEX_POINT('',#36714);
#11473=VERTEX_POINT('',#36716);
#11474=VERTEX_POINT('',#36720);
#11475=VERTEX_POINT('',#36722);
#11476=VERTEX_POINT('',#36724);
#11477=VERTEX_POINT('',#36728);
#11478=VERTEX_POINT('',#36732);
#11479=VERTEX_POINT('',#36734);
#11480=VERTEX_POINT('',#36736);
#11481=VERTEX_POINT('',#36738);
#11482=VERTEX_POINT('',#36742);
#11483=VERTEX_POINT('',#36744);
#11484=VERTEX_POINT('',#36746);
#11485=VERTEX_POINT('',#36750);
#11486=VERTEX_POINT('',#36754);
#11487=VERTEX_POINT('',#36756);
#11488=VERTEX_POINT('',#36758);
#11489=VERTEX_POINT('',#36760);
#11490=VERTEX_POINT('',#36764);
#11491=VERTEX_POINT('',#36766);
#11492=VERTEX_POINT('',#36768);
#11493=VERTEX_POINT('',#36772);
#11494=VERTEX_POINT('',#36776);
#11495=VERTEX_POINT('',#36777);
#11496=VERTEX_POINT('',#36779);
#11497=VERTEX_POINT('',#36782);
#11498=VERTEX_POINT('',#36786);
#11499=VERTEX_POINT('',#36788);
#11500=VERTEX_POINT('',#36792);
#11501=VERTEX_POINT('',#36796);
#11502=VERTEX_POINT('',#36797);
#11503=VERTEX_POINT('',#36799);
#11504=VERTEX_POINT('',#36802);
#11505=VERTEX_POINT('',#36806);
#11506=VERTEX_POINT('',#36808);
#11507=VERTEX_POINT('',#36812);
#11508=VERTEX_POINT('',#36816);
#11509=VERTEX_POINT('',#36817);
#11510=VERTEX_POINT('',#36819);
#11511=VERTEX_POINT('',#36822);
#11512=VERTEX_POINT('',#36826);
#11513=VERTEX_POINT('',#36828);
#11514=VERTEX_POINT('',#36832);
#11515=VERTEX_POINT('',#36836);
#11516=VERTEX_POINT('',#36837);
#11517=VERTEX_POINT('',#36839);
#11518=VERTEX_POINT('',#36842);
#11519=VERTEX_POINT('',#36846);
#11520=VERTEX_POINT('',#36848);
#11521=VERTEX_POINT('',#36852);
#11522=VERTEX_POINT('',#36856);
#11523=VERTEX_POINT('',#36857);
#11524=VERTEX_POINT('',#36859);
#11525=VERTEX_POINT('',#36862);
#11526=VERTEX_POINT('',#36866);
#11527=VERTEX_POINT('',#36868);
#11528=VERTEX_POINT('',#36872);
#11529=VERTEX_POINT('',#36876);
#11530=VERTEX_POINT('',#36877);
#11531=VERTEX_POINT('',#36879);
#11532=VERTEX_POINT('',#36882);
#11533=VERTEX_POINT('',#36886);
#11534=VERTEX_POINT('',#36888);
#11535=VERTEX_POINT('',#36892);
#11536=VERTEX_POINT('',#36896);
#11537=VERTEX_POINT('',#36897);
#11538=VERTEX_POINT('',#36899);
#11539=VERTEX_POINT('',#36902);
#11540=VERTEX_POINT('',#36906);
#11541=VERTEX_POINT('',#36908);
#11542=VERTEX_POINT('',#36912);
#11543=VERTEX_POINT('',#36916);
#11544=VERTEX_POINT('',#36917);
#11545=VERTEX_POINT('',#36919);
#11546=VERTEX_POINT('',#36922);
#11547=VERTEX_POINT('',#36926);
#11548=VERTEX_POINT('',#36928);
#11549=VERTEX_POINT('',#36932);
#11550=VERTEX_POINT('',#36936);
#11551=VERTEX_POINT('',#36937);
#11552=VERTEX_POINT('',#36939);
#11553=VERTEX_POINT('',#36942);
#11554=VERTEX_POINT('',#36946);
#11555=VERTEX_POINT('',#36948);
#11556=VERTEX_POINT('',#36952);
#11557=VERTEX_POINT('',#36956);
#11558=VERTEX_POINT('',#36957);
#11559=VERTEX_POINT('',#36959);
#11560=VERTEX_POINT('',#36962);
#11561=VERTEX_POINT('',#36966);
#11562=VERTEX_POINT('',#36968);
#11563=VERTEX_POINT('',#36972);
#11564=VERTEX_POINT('',#36976);
#11565=VERTEX_POINT('',#36977);
#11566=VERTEX_POINT('',#36979);
#11567=VERTEX_POINT('',#36982);
#11568=VERTEX_POINT('',#36986);
#11569=VERTEX_POINT('',#36988);
#11570=VERTEX_POINT('',#36992);
#11571=VERTEX_POINT('',#36996);
#11572=VERTEX_POINT('',#36997);
#11573=VERTEX_POINT('',#36999);
#11574=VERTEX_POINT('',#37002);
#11575=VERTEX_POINT('',#37006);
#11576=VERTEX_POINT('',#37008);
#11577=VERTEX_POINT('',#37012);
#11578=VERTEX_POINT('',#37016);
#11579=VERTEX_POINT('',#37018);
#11580=VERTEX_POINT('',#37020);
#11581=VERTEX_POINT('',#37024);
#11582=VERTEX_POINT('',#37026);
#11583=VERTEX_POINT('',#37028);
#11584=VERTEX_POINT('',#37030);
#11585=VERTEX_POINT('',#37032);
#11586=VERTEX_POINT('',#37034);
#11587=VERTEX_POINT('',#37036);
#11588=VERTEX_POINT('',#37038);
#11589=VERTEX_POINT('',#37040);
#11590=VERTEX_POINT('',#37042);
#11591=VERTEX_POINT('',#37044);
#11592=VERTEX_POINT('',#37046);
#11593=VERTEX_POINT('',#37048);
#11594=VERTEX_POINT('',#37050);
#11595=VERTEX_POINT('',#37052);
#11596=VERTEX_POINT('',#37054);
#11597=VERTEX_POINT('',#37056);
#11598=VERTEX_POINT('',#37059);
#11599=VERTEX_POINT('',#37061);
#11600=VERTEX_POINT('',#37063);
#11601=VERTEX_POINT('',#37065);
#11602=VERTEX_POINT('',#37067);
#11603=VERTEX_POINT('',#37069);
#11604=VERTEX_POINT('',#37071);
#11605=VERTEX_POINT('',#37073);
#11606=VERTEX_POINT('',#37075);
#11607=VERTEX_POINT('',#37077);
#11608=VERTEX_POINT('',#37079);
#11609=VERTEX_POINT('',#37081);
#11610=VERTEX_POINT('',#37083);
#11611=VERTEX_POINT('',#37085);
#11612=VERTEX_POINT('',#37087);
#11613=VERTEX_POINT('',#37089);
#11614=VERTEX_POINT('',#37091);
#11615=VERTEX_POINT('',#37093);
#11616=VERTEX_POINT('',#37096);
#11617=VERTEX_POINT('',#37098);
#11618=VERTEX_POINT('',#37100);
#11619=VERTEX_POINT('',#37102);
#11620=VERTEX_POINT('',#37104);
#11621=VERTEX_POINT('',#37106);
#11622=VERTEX_POINT('',#37108);
#11623=VERTEX_POINT('',#37110);
#11624=VERTEX_POINT('',#37112);
#11625=VERTEX_POINT('',#37114);
#11626=VERTEX_POINT('',#37116);
#11627=VERTEX_POINT('',#37118);
#11628=VERTEX_POINT('',#37120);
#11629=VERTEX_POINT('',#37122);
#11630=VERTEX_POINT('',#37124);
#11631=VERTEX_POINT('',#37126);
#11632=VERTEX_POINT('',#37128);
#11633=VERTEX_POINT('',#37130);
#11634=VERTEX_POINT('',#37133);
#11635=VERTEX_POINT('',#37135);
#11636=VERTEX_POINT('',#37137);
#11637=VERTEX_POINT('',#37139);
#11638=VERTEX_POINT('',#37141);
#11639=VERTEX_POINT('',#37143);
#11640=VERTEX_POINT('',#37145);
#11641=VERTEX_POINT('',#37147);
#11642=VERTEX_POINT('',#37149);
#11643=VERTEX_POINT('',#37151);
#11644=VERTEX_POINT('',#37153);
#11645=VERTEX_POINT('',#37155);
#11646=VERTEX_POINT('',#37157);
#11647=VERTEX_POINT('',#37159);
#11648=VERTEX_POINT('',#37161);
#11649=VERTEX_POINT('',#37163);
#11650=VERTEX_POINT('',#37165);
#11651=VERTEX_POINT('',#37167);
#11652=VERTEX_POINT('',#37170);
#11653=VERTEX_POINT('',#37172);
#11654=VERTEX_POINT('',#37174);
#11655=VERTEX_POINT('',#37176);
#11656=VERTEX_POINT('',#37178);
#11657=VERTEX_POINT('',#37180);
#11658=VERTEX_POINT('',#37182);
#11659=VERTEX_POINT('',#37184);
#11660=VERTEX_POINT('',#37186);
#11661=VERTEX_POINT('',#37188);
#11662=VERTEX_POINT('',#37190);
#11663=VERTEX_POINT('',#37192);
#11664=VERTEX_POINT('',#37194);
#11665=VERTEX_POINT('',#37196);
#11666=VERTEX_POINT('',#37198);
#11667=VERTEX_POINT('',#37200);
#11668=VERTEX_POINT('',#37202);
#11669=VERTEX_POINT('',#37204);
#11670=VERTEX_POINT('',#37207);
#11671=VERTEX_POINT('',#37209);
#11672=VERTEX_POINT('',#37211);
#11673=VERTEX_POINT('',#37213);
#11674=VERTEX_POINT('',#37215);
#11675=VERTEX_POINT('',#37217);
#11676=VERTEX_POINT('',#37219);
#11677=VERTEX_POINT('',#37221);
#11678=VERTEX_POINT('',#37223);
#11679=VERTEX_POINT('',#37225);
#11680=VERTEX_POINT('',#37227);
#11681=VERTEX_POINT('',#37229);
#11682=VERTEX_POINT('',#37231);
#11683=VERTEX_POINT('',#37233);
#11684=VERTEX_POINT('',#37235);
#11685=VERTEX_POINT('',#37237);
#11686=VERTEX_POINT('',#37239);
#11687=VERTEX_POINT('',#37241);
#11688=VERTEX_POINT('',#37244);
#11689=VERTEX_POINT('',#37246);
#11690=VERTEX_POINT('',#37248);
#11691=VERTEX_POINT('',#37250);
#11692=VERTEX_POINT('',#37252);
#11693=VERTEX_POINT('',#37254);
#11694=VERTEX_POINT('',#37256);
#11695=VERTEX_POINT('',#37258);
#11696=VERTEX_POINT('',#37260);
#11697=VERTEX_POINT('',#37262);
#11698=VERTEX_POINT('',#37264);
#11699=VERTEX_POINT('',#37266);
#11700=VERTEX_POINT('',#37268);
#11701=VERTEX_POINT('',#37270);
#11702=VERTEX_POINT('',#37272);
#11703=VERTEX_POINT('',#37274);
#11704=VERTEX_POINT('',#37276);
#11705=VERTEX_POINT('',#37278);
#11706=VERTEX_POINT('',#37281);
#11707=VERTEX_POINT('',#37283);
#11708=VERTEX_POINT('',#37285);
#11709=VERTEX_POINT('',#37287);
#11710=VERTEX_POINT('',#37289);
#11711=VERTEX_POINT('',#37291);
#11712=VERTEX_POINT('',#37293);
#11713=VERTEX_POINT('',#37295);
#11714=VERTEX_POINT('',#37297);
#11715=VERTEX_POINT('',#37299);
#11716=VERTEX_POINT('',#37301);
#11717=VERTEX_POINT('',#37303);
#11718=VERTEX_POINT('',#37305);
#11719=VERTEX_POINT('',#37307);
#11720=VERTEX_POINT('',#37309);
#11721=VERTEX_POINT('',#37311);
#11722=VERTEX_POINT('',#37313);
#11723=VERTEX_POINT('',#37315);
#11724=VERTEX_POINT('',#37318);
#11725=VERTEX_POINT('',#37320);
#11726=VERTEX_POINT('',#37322);
#11727=VERTEX_POINT('',#37324);
#11728=VERTEX_POINT('',#37326);
#11729=VERTEX_POINT('',#37328);
#11730=VERTEX_POINT('',#37330);
#11731=VERTEX_POINT('',#37332);
#11732=VERTEX_POINT('',#37334);
#11733=VERTEX_POINT('',#37336);
#11734=VERTEX_POINT('',#37338);
#11735=VERTEX_POINT('',#37340);
#11736=VERTEX_POINT('',#37342);
#11737=VERTEX_POINT('',#37344);
#11738=VERTEX_POINT('',#37346);
#11739=VERTEX_POINT('',#37348);
#11740=VERTEX_POINT('',#37350);
#11741=VERTEX_POINT('',#37352);
#11742=VERTEX_POINT('',#37355);
#11743=VERTEX_POINT('',#37357);
#11744=VERTEX_POINT('',#37359);
#11745=VERTEX_POINT('',#37361);
#11746=VERTEX_POINT('',#37363);
#11747=VERTEX_POINT('',#37365);
#11748=VERTEX_POINT('',#37367);
#11749=VERTEX_POINT('',#37369);
#11750=VERTEX_POINT('',#37371);
#11751=VERTEX_POINT('',#37373);
#11752=VERTEX_POINT('',#37375);
#11753=VERTEX_POINT('',#37377);
#11754=VERTEX_POINT('',#37379);
#11755=VERTEX_POINT('',#37381);
#11756=VERTEX_POINT('',#37383);
#11757=VERTEX_POINT('',#37385);
#11758=VERTEX_POINT('',#37387);
#11759=VERTEX_POINT('',#37389);
#11760=VERTEX_POINT('',#37392);
#11761=VERTEX_POINT('',#37394);
#11762=VERTEX_POINT('',#37396);
#11763=VERTEX_POINT('',#37398);
#11764=VERTEX_POINT('',#37400);
#11765=VERTEX_POINT('',#37402);
#11766=VERTEX_POINT('',#37404);
#11767=VERTEX_POINT('',#37406);
#11768=VERTEX_POINT('',#37408);
#11769=VERTEX_POINT('',#37410);
#11770=VERTEX_POINT('',#37412);
#11771=VERTEX_POINT('',#37414);
#11772=VERTEX_POINT('',#37416);
#11773=VERTEX_POINT('',#37418);
#11774=VERTEX_POINT('',#37420);
#11775=VERTEX_POINT('',#37422);
#11776=VERTEX_POINT('',#37424);
#11777=VERTEX_POINT('',#37426);
#11778=VERTEX_POINT('',#37429);
#11779=VERTEX_POINT('',#37431);
#11780=VERTEX_POINT('',#37433);
#11781=VERTEX_POINT('',#37435);
#11782=VERTEX_POINT('',#37437);
#11783=VERTEX_POINT('',#37439);
#11784=VERTEX_POINT('',#37441);
#11785=VERTEX_POINT('',#37443);
#11786=VERTEX_POINT('',#37445);
#11787=VERTEX_POINT('',#37447);
#11788=VERTEX_POINT('',#37449);
#11789=VERTEX_POINT('',#37451);
#11790=VERTEX_POINT('',#37453);
#11791=VERTEX_POINT('',#37455);
#11792=VERTEX_POINT('',#37457);
#11793=VERTEX_POINT('',#37459);
#11794=VERTEX_POINT('',#37461);
#11795=VERTEX_POINT('',#37463);
#11796=VERTEX_POINT('',#37466);
#11797=VERTEX_POINT('',#37469);
#11798=VERTEX_POINT('',#37474);
#11799=VERTEX_POINT('',#37476);
#11800=VERTEX_POINT('',#37480);
#11801=VERTEX_POINT('',#37485);
#11802=VERTEX_POINT('',#37487);
#11803=VERTEX_POINT('',#37491);
#11804=VERTEX_POINT('',#37496);
#11805=VERTEX_POINT('',#37498);
#11806=VERTEX_POINT('',#37502);
#11807=VERTEX_POINT('',#37507);
#11808=VERTEX_POINT('',#37509);
#11809=VERTEX_POINT('',#37513);
#11810=VERTEX_POINT('',#37518);
#11811=VERTEX_POINT('',#37520);
#11812=VERTEX_POINT('',#37524);
#11813=VERTEX_POINT('',#37529);
#11814=VERTEX_POINT('',#37531);
#11815=VERTEX_POINT('',#37535);
#11816=VERTEX_POINT('',#37540);
#11817=VERTEX_POINT('',#37542);
#11818=VERTEX_POINT('',#37546);
#11819=VERTEX_POINT('',#37551);
#11820=VERTEX_POINT('',#37553);
#11821=VERTEX_POINT('',#37557);
#11822=VERTEX_POINT('',#37562);
#11823=VERTEX_POINT('',#37564);
#11824=VERTEX_POINT('',#37568);
#11825=VERTEX_POINT('',#37573);
#11826=VERTEX_POINT('',#37575);
#11827=VERTEX_POINT('',#37579);
#11828=VERTEX_POINT('',#37584);
#11829=VERTEX_POINT('',#37586);
#11830=VERTEX_POINT('',#37590);
#11831=VERTEX_POINT('',#37595);
#11832=VERTEX_POINT('',#37596);
#11833=VERTEX_POINT('',#37598);
#11834=VERTEX_POINT('',#37600);
#11835=VERTEX_POINT('',#37604);
#11836=VERTEX_POINT('',#37606);
#11837=VERTEX_POINT('',#37610);
#11838=VERTEX_POINT('',#37612);
#11839=VERTEX_POINT('',#38076);
#11840=VERTEX_POINT('',#38080);
#11841=VERTEX_POINT('',#38083);
#11842=VERTEX_POINT('',#38087);
#11843=VERTEX_POINT('',#38092);
#11844=VERTEX_POINT('',#38098);
#11845=VERTEX_POINT('',#38099);
#11846=VERTEX_POINT('',#38101);
#11847=VERTEX_POINT('',#38103);
#11848=VERTEX_POINT('',#38105);
#11849=VERTEX_POINT('',#38107);
#11850=VERTEX_POINT('',#38111);
#11851=VERTEX_POINT('',#38113);
#11852=VERTEX_POINT('',#38115);
#11853=VERTEX_POINT('',#38117);
#11854=VERTEX_POINT('',#38119);
#11855=VERTEX_POINT('',#38121);
#11856=VERTEX_POINT('',#38123);
#11857=VERTEX_POINT('',#38125);
#11858=VERTEX_POINT('',#38127);
#11859=VERTEX_POINT('',#38129);
#11860=VERTEX_POINT('',#38131);
#11861=VERTEX_POINT('',#38133);
#11862=VERTEX_POINT('',#38135);
#11863=VERTEX_POINT('',#38137);
#11864=VERTEX_POINT('',#38139);
#11865=VERTEX_POINT('',#38141);
#11866=VERTEX_POINT('',#38143);
#11867=VERTEX_POINT('',#38145);
#11868=VERTEX_POINT('',#38147);
#11869=VERTEX_POINT('',#38149);
#11870=VERTEX_POINT('',#38151);
#11871=VERTEX_POINT('',#38153);
#11872=VERTEX_POINT('',#38155);
#11873=VERTEX_POINT('',#38157);
#11874=VERTEX_POINT('',#38159);
#11875=VERTEX_POINT('',#38161);
#11876=VERTEX_POINT('',#38163);
#11877=VERTEX_POINT('',#38165);
#11878=VERTEX_POINT('',#38167);
#11879=VERTEX_POINT('',#38169);
#11880=VERTEX_POINT('',#38171);
#11881=VERTEX_POINT('',#38173);
#11882=VERTEX_POINT('',#38175);
#11883=VERTEX_POINT('',#38177);
#11884=VERTEX_POINT('',#38179);
#11885=VERTEX_POINT('',#38181);
#11886=VERTEX_POINT('',#38183);
#11887=VERTEX_POINT('',#38185);
#11888=VERTEX_POINT('',#38187);
#11889=VERTEX_POINT('',#38189);
#11890=VERTEX_POINT('',#38191);
#11891=VERTEX_POINT('',#38193);
#11892=VERTEX_POINT('',#38195);
#11893=VERTEX_POINT('',#38197);
#11894=VERTEX_POINT('',#38199);
#11895=VERTEX_POINT('',#38201);
#11896=VERTEX_POINT('',#38203);
#11897=VERTEX_POINT('',#38205);
#11898=VERTEX_POINT('',#38207);
#11899=VERTEX_POINT('',#38209);
#11900=VERTEX_POINT('',#38211);
#11901=VERTEX_POINT('',#38213);
#11902=VERTEX_POINT('',#38215);
#11903=VERTEX_POINT('',#38217);
#11904=VERTEX_POINT('',#38219);
#11905=VERTEX_POINT('',#38221);
#11906=VERTEX_POINT('',#38223);
#11907=VERTEX_POINT('',#38225);
#11908=VERTEX_POINT('',#38227);
#11909=VERTEX_POINT('',#38229);
#11910=VERTEX_POINT('',#38231);
#11911=VERTEX_POINT('',#38233);
#11912=VERTEX_POINT('',#38235);
#11913=VERTEX_POINT('',#38237);
#11914=VERTEX_POINT('',#38239);
#11915=VERTEX_POINT('',#38241);
#11916=VERTEX_POINT('',#38243);
#11917=VERTEX_POINT('',#38245);
#11918=VERTEX_POINT('',#38247);
#11919=VERTEX_POINT('',#38249);
#11920=VERTEX_POINT('',#38251);
#11921=VERTEX_POINT('',#38253);
#11922=VERTEX_POINT('',#38255);
#11923=VERTEX_POINT('',#38257);
#11924=VERTEX_POINT('',#38259);
#11925=VERTEX_POINT('',#38261);
#11926=VERTEX_POINT('',#38263);
#11927=VERTEX_POINT('',#38265);
#11928=VERTEX_POINT('',#38267);
#11929=VERTEX_POINT('',#38269);
#11930=VERTEX_POINT('',#38271);
#11931=VERTEX_POINT('',#38273);
#11932=VERTEX_POINT('',#38275);
#11933=VERTEX_POINT('',#38277);
#11934=VERTEX_POINT('',#38279);
#11935=VERTEX_POINT('',#38281);
#11936=VERTEX_POINT('',#38283);
#11937=VERTEX_POINT('',#38285);
#11938=VERTEX_POINT('',#38287);
#11939=VERTEX_POINT('',#38289);
#11940=VERTEX_POINT('',#38291);
#11941=VERTEX_POINT('',#38293);
#11942=VERTEX_POINT('',#38295);
#11943=VERTEX_POINT('',#38297);
#11944=VERTEX_POINT('',#38299);
#11945=VERTEX_POINT('',#38301);
#11946=VERTEX_POINT('',#38303);
#11947=VERTEX_POINT('',#38305);
#11948=VERTEX_POINT('',#38307);
#11949=VERTEX_POINT('',#38309);
#11950=VERTEX_POINT('',#38311);
#11951=VERTEX_POINT('',#38313);
#11952=VERTEX_POINT('',#38315);
#11953=VERTEX_POINT('',#38317);
#11954=VERTEX_POINT('',#38319);
#11955=VERTEX_POINT('',#38321);
#11956=VERTEX_POINT('',#38323);
#11957=VERTEX_POINT('',#38325);
#11958=VERTEX_POINT('',#38327);
#11959=VERTEX_POINT('',#38329);
#11960=VERTEX_POINT('',#38331);
#11961=VERTEX_POINT('',#38333);
#11962=VERTEX_POINT('',#38335);
#11963=VERTEX_POINT('',#38337);
#11964=VERTEX_POINT('',#38339);
#11965=VERTEX_POINT('',#38341);
#11966=VERTEX_POINT('',#38343);
#11967=VERTEX_POINT('',#38345);
#11968=VERTEX_POINT('',#38347);
#11969=VERTEX_POINT('',#38349);
#11970=VERTEX_POINT('',#38351);
#11971=VERTEX_POINT('',#38353);
#11972=VERTEX_POINT('',#38355);
#11973=VERTEX_POINT('',#38357);
#11974=VERTEX_POINT('',#38359);
#11975=VERTEX_POINT('',#38361);
#11976=VERTEX_POINT('',#38363);
#11977=VERTEX_POINT('',#38365);
#11978=VERTEX_POINT('',#38367);
#11979=VERTEX_POINT('',#38369);
#11980=VERTEX_POINT('',#38371);
#11981=VERTEX_POINT('',#38373);
#11982=VERTEX_POINT('',#38375);
#11983=VERTEX_POINT('',#38377);
#11984=VERTEX_POINT('',#38379);
#11985=VERTEX_POINT('',#38381);
#11986=VERTEX_POINT('',#38383);
#11987=VERTEX_POINT('',#38385);
#11988=VERTEX_POINT('',#38387);
#11989=VERTEX_POINT('',#38389);
#11990=VERTEX_POINT('',#38391);
#11991=VERTEX_POINT('',#38393);
#11992=VERTEX_POINT('',#38395);
#11993=VERTEX_POINT('',#38397);
#11994=VERTEX_POINT('',#38399);
#11995=VERTEX_POINT('',#38401);
#11996=VERTEX_POINT('',#38403);
#11997=VERTEX_POINT('',#38405);
#11998=VERTEX_POINT('',#38407);
#11999=VERTEX_POINT('',#38409);
#12000=VERTEX_POINT('',#38411);
#12001=VERTEX_POINT('',#38413);
#12002=VERTEX_POINT('',#38415);
#12003=VERTEX_POINT('',#38417);
#12004=VERTEX_POINT('',#38419);
#12005=VERTEX_POINT('',#38421);
#12006=VERTEX_POINT('',#38423);
#12007=VERTEX_POINT('',#38425);
#12008=VERTEX_POINT('',#38427);
#12009=VERTEX_POINT('',#38429);
#12010=VERTEX_POINT('',#38431);
#12011=VERTEX_POINT('',#38433);
#12012=VERTEX_POINT('',#38435);
#12013=VERTEX_POINT('',#38437);
#12014=VERTEX_POINT('',#38439);
#12015=VERTEX_POINT('',#38441);
#12016=VERTEX_POINT('',#38443);
#12017=VERTEX_POINT('',#38445);
#12018=VERTEX_POINT('',#38447);
#12019=VERTEX_POINT('',#38449);
#12020=VERTEX_POINT('',#38451);
#12021=VERTEX_POINT('',#38453);
#12022=VERTEX_POINT('',#38455);
#12023=VERTEX_POINT('',#38457);
#12024=VERTEX_POINT('',#38459);
#12025=VERTEX_POINT('',#38461);
#12026=VERTEX_POINT('',#38463);
#12027=VERTEX_POINT('',#38465);
#12028=VERTEX_POINT('',#38467);
#12029=VERTEX_POINT('',#38469);
#12030=VERTEX_POINT('',#38471);
#12031=VERTEX_POINT('',#38473);
#12032=VERTEX_POINT('',#38475);
#12033=VERTEX_POINT('',#38477);
#12034=VERTEX_POINT('',#38479);
#12035=VERTEX_POINT('',#38481);
#12036=VERTEX_POINT('',#38483);
#12037=VERTEX_POINT('',#38485);
#12038=VERTEX_POINT('',#38487);
#12039=VERTEX_POINT('',#38489);
#12040=VERTEX_POINT('',#38491);
#12041=VERTEX_POINT('',#38493);
#12042=VERTEX_POINT('',#38495);
#12043=VERTEX_POINT('',#38497);
#12044=VERTEX_POINT('',#38499);
#12045=VERTEX_POINT('',#38501);
#12046=VERTEX_POINT('',#38503);
#12047=VERTEX_POINT('',#38505);
#12048=VERTEX_POINT('',#38507);
#12049=VERTEX_POINT('',#38509);
#12050=VERTEX_POINT('',#38511);
#12051=VERTEX_POINT('',#38513);
#12052=VERTEX_POINT('',#38515);
#12053=VERTEX_POINT('',#38517);
#12054=VERTEX_POINT('',#38519);
#12055=VERTEX_POINT('',#38521);
#12056=VERTEX_POINT('',#38523);
#12057=VERTEX_POINT('',#38525);
#12058=VERTEX_POINT('',#38527);
#12059=VERTEX_POINT('',#38529);
#12060=VERTEX_POINT('',#38531);
#12061=VERTEX_POINT('',#38533);
#12062=VERTEX_POINT('',#38535);
#12063=VERTEX_POINT('',#38537);
#12064=VERTEX_POINT('',#38539);
#12065=VERTEX_POINT('',#38541);
#12066=VERTEX_POINT('',#38543);
#12067=VERTEX_POINT('',#38545);
#12068=VERTEX_POINT('',#38547);
#12069=VERTEX_POINT('',#38549);
#12070=VERTEX_POINT('',#38551);
#12071=VERTEX_POINT('',#38553);
#12072=VERTEX_POINT('',#38555);
#12073=VERTEX_POINT('',#38557);
#12074=VERTEX_POINT('',#38559);
#12075=VERTEX_POINT('',#38561);
#12076=VERTEX_POINT('',#38563);
#12077=VERTEX_POINT('',#38565);
#12078=VERTEX_POINT('',#38567);
#12079=VERTEX_POINT('',#38569);
#12080=VERTEX_POINT('',#38571);
#12081=VERTEX_POINT('',#38573);
#12082=VERTEX_POINT('',#38575);
#12083=VERTEX_POINT('',#38577);
#12084=VERTEX_POINT('',#38579);
#12085=VERTEX_POINT('',#38581);
#12086=VERTEX_POINT('',#38583);
#12087=VERTEX_POINT('',#38585);
#12088=VERTEX_POINT('',#38588);
#12089=VERTEX_POINT('',#38591);
#12090=VERTEX_POINT('',#38593);
#12091=VERTEX_POINT('',#38595);
#12092=VERTEX_POINT('',#38599);
#12093=VERTEX_POINT('',#38603);
#12094=VERTEX_POINT('',#38605);
#12095=VERTEX_POINT('',#38607);
#12096=VERTEX_POINT('',#38609);
#12097=VERTEX_POINT('',#38613);
#12098=VERTEX_POINT('',#38615);
#12099=VERTEX_POINT('',#38617);
#12100=VERTEX_POINT('',#38621);
#12101=VERTEX_POINT('',#38625);
#12102=VERTEX_POINT('',#38627);
#12103=VERTEX_POINT('',#38629);
#12104=VERTEX_POINT('',#38631);
#12105=VERTEX_POINT('',#38635);
#12106=VERTEX_POINT('',#38637);
#12107=VERTEX_POINT('',#38639);
#12108=VERTEX_POINT('',#38643);
#12109=VERTEX_POINT('',#38647);
#12110=VERTEX_POINT('',#38649);
#12111=VERTEX_POINT('',#38651);
#12112=VERTEX_POINT('',#38653);
#12113=VERTEX_POINT('',#38657);
#12114=VERTEX_POINT('',#38659);
#12115=VERTEX_POINT('',#38661);
#12116=VERTEX_POINT('',#38665);
#12117=VERTEX_POINT('',#38669);
#12118=VERTEX_POINT('',#38671);
#12119=VERTEX_POINT('',#38673);
#12120=VERTEX_POINT('',#38675);
#12121=VERTEX_POINT('',#38679);
#12122=VERTEX_POINT('',#38681);
#12123=VERTEX_POINT('',#38683);
#12124=VERTEX_POINT('',#38687);
#12125=VERTEX_POINT('',#38691);
#12126=VERTEX_POINT('',#38693);
#12127=VERTEX_POINT('',#38695);
#12128=VERTEX_POINT('',#38697);
#12129=VERTEX_POINT('',#38701);
#12130=VERTEX_POINT('',#38703);
#12131=VERTEX_POINT('',#38705);
#12132=VERTEX_POINT('',#38709);
#12133=VERTEX_POINT('',#38713);
#12134=VERTEX_POINT('',#38715);
#12135=VERTEX_POINT('',#38717);
#12136=VERTEX_POINT('',#38719);
#12137=VERTEX_POINT('',#38723);
#12138=VERTEX_POINT('',#38725);
#12139=VERTEX_POINT('',#38727);
#12140=VERTEX_POINT('',#38731);
#12141=VERTEX_POINT('',#38735);
#12142=VERTEX_POINT('',#38737);
#12143=VERTEX_POINT('',#38739);
#12144=VERTEX_POINT('',#38741);
#12145=VERTEX_POINT('',#38745);
#12146=VERTEX_POINT('',#38747);
#12147=VERTEX_POINT('',#38749);
#12148=VERTEX_POINT('',#38753);
#12149=VERTEX_POINT('',#38757);
#12150=VERTEX_POINT('',#38759);
#12151=VERTEX_POINT('',#38761);
#12152=VERTEX_POINT('',#38763);
#12153=VERTEX_POINT('',#38767);
#12154=VERTEX_POINT('',#38769);
#12155=VERTEX_POINT('',#38771);
#12156=VERTEX_POINT('',#38775);
#12157=VERTEX_POINT('',#38779);
#12158=VERTEX_POINT('',#38781);
#12159=VERTEX_POINT('',#38783);
#12160=VERTEX_POINT('',#38785);
#12161=VERTEX_POINT('',#38789);
#12162=VERTEX_POINT('',#38791);
#12163=VERTEX_POINT('',#38793);
#12164=VERTEX_POINT('',#38797);
#12165=VERTEX_POINT('',#38801);
#12166=VERTEX_POINT('',#38803);
#12167=VERTEX_POINT('',#38805);
#12168=VERTEX_POINT('',#38807);
#12169=VERTEX_POINT('',#38811);
#12170=VERTEX_POINT('',#38813);
#12171=VERTEX_POINT('',#38815);
#12172=VERTEX_POINT('',#38819);
#12173=VERTEX_POINT('',#38823);
#12174=VERTEX_POINT('',#38825);
#12175=VERTEX_POINT('',#38827);
#12176=VERTEX_POINT('',#38829);
#12177=VERTEX_POINT('',#38833);
#12178=VERTEX_POINT('',#38835);
#12179=VERTEX_POINT('',#38837);
#12180=VERTEX_POINT('',#38841);
#12181=VERTEX_POINT('',#38845);
#12182=VERTEX_POINT('',#38846);
#12183=VERTEX_POINT('',#38848);
#12184=VERTEX_POINT('',#38851);
#12185=VERTEX_POINT('',#38855);
#12186=VERTEX_POINT('',#38857);
#12187=VERTEX_POINT('',#38861);
#12188=VERTEX_POINT('',#38865);
#12189=VERTEX_POINT('',#38866);
#12190=VERTEX_POINT('',#38868);
#12191=VERTEX_POINT('',#38871);
#12192=VERTEX_POINT('',#38875);
#12193=VERTEX_POINT('',#38877);
#12194=VERTEX_POINT('',#38881);
#12195=VERTEX_POINT('',#38885);
#12196=VERTEX_POINT('',#38886);
#12197=VERTEX_POINT('',#38888);
#12198=VERTEX_POINT('',#38891);
#12199=VERTEX_POINT('',#38895);
#12200=VERTEX_POINT('',#38897);
#12201=VERTEX_POINT('',#38901);
#12202=VERTEX_POINT('',#38905);
#12203=VERTEX_POINT('',#38906);
#12204=VERTEX_POINT('',#38908);
#12205=VERTEX_POINT('',#38911);
#12206=VERTEX_POINT('',#38915);
#12207=VERTEX_POINT('',#38917);
#12208=VERTEX_POINT('',#38921);
#12209=VERTEX_POINT('',#38925);
#12210=VERTEX_POINT('',#38926);
#12211=VERTEX_POINT('',#38928);
#12212=VERTEX_POINT('',#38931);
#12213=VERTEX_POINT('',#38935);
#12214=VERTEX_POINT('',#38937);
#12215=VERTEX_POINT('',#38941);
#12216=VERTEX_POINT('',#38945);
#12217=VERTEX_POINT('',#38946);
#12218=VERTEX_POINT('',#38948);
#12219=VERTEX_POINT('',#38951);
#12220=VERTEX_POINT('',#38955);
#12221=VERTEX_POINT('',#38957);
#12222=VERTEX_POINT('',#38961);
#12223=VERTEX_POINT('',#38965);
#12224=VERTEX_POINT('',#38966);
#12225=VERTEX_POINT('',#38968);
#12226=VERTEX_POINT('',#38971);
#12227=VERTEX_POINT('',#38975);
#12228=VERTEX_POINT('',#38977);
#12229=VERTEX_POINT('',#38981);
#12230=VERTEX_POINT('',#38985);
#12231=VERTEX_POINT('',#38986);
#12232=VERTEX_POINT('',#38988);
#12233=VERTEX_POINT('',#38991);
#12234=VERTEX_POINT('',#38995);
#12235=VERTEX_POINT('',#38997);
#12236=VERTEX_POINT('',#39001);
#12237=VERTEX_POINT('',#39005);
#12238=VERTEX_POINT('',#39006);
#12239=VERTEX_POINT('',#39008);
#12240=VERTEX_POINT('',#39011);
#12241=VERTEX_POINT('',#39015);
#12242=VERTEX_POINT('',#39017);
#12243=VERTEX_POINT('',#39021);
#12244=VERTEX_POINT('',#39025);
#12245=VERTEX_POINT('',#39026);
#12246=VERTEX_POINT('',#39028);
#12247=VERTEX_POINT('',#39031);
#12248=VERTEX_POINT('',#39035);
#12249=VERTEX_POINT('',#39037);
#12250=VERTEX_POINT('',#39041);
#12251=VERTEX_POINT('',#39045);
#12252=VERTEX_POINT('',#39046);
#12253=VERTEX_POINT('',#39048);
#12254=VERTEX_POINT('',#39051);
#12255=VERTEX_POINT('',#39055);
#12256=VERTEX_POINT('',#39057);
#12257=VERTEX_POINT('',#39061);
#12258=VERTEX_POINT('',#39065);
#12259=VERTEX_POINT('',#39066);
#12260=VERTEX_POINT('',#39068);
#12261=VERTEX_POINT('',#39071);
#12262=VERTEX_POINT('',#39075);
#12263=VERTEX_POINT('',#39077);
#12264=VERTEX_POINT('',#39081);
#12265=VERTEX_POINT('',#39085);
#12266=VERTEX_POINT('',#39087);
#12267=VERTEX_POINT('',#39089);
#12268=VERTEX_POINT('',#39093);
#12269=VERTEX_POINT('',#39095);
#12270=VERTEX_POINT('',#39097);
#12271=VERTEX_POINT('',#39099);
#12272=VERTEX_POINT('',#39101);
#12273=VERTEX_POINT('',#39103);
#12274=VERTEX_POINT('',#39105);
#12275=VERTEX_POINT('',#39107);
#12276=VERTEX_POINT('',#39109);
#12277=VERTEX_POINT('',#39111);
#12278=VERTEX_POINT('',#39113);
#12279=VERTEX_POINT('',#39115);
#12280=VERTEX_POINT('',#39117);
#12281=VERTEX_POINT('',#39119);
#12282=VERTEX_POINT('',#39121);
#12283=VERTEX_POINT('',#39123);
#12284=VERTEX_POINT('',#39125);
#12285=VERTEX_POINT('',#39128);
#12286=VERTEX_POINT('',#39130);
#12287=VERTEX_POINT('',#39132);
#12288=VERTEX_POINT('',#39134);
#12289=VERTEX_POINT('',#39136);
#12290=VERTEX_POINT('',#39138);
#12291=VERTEX_POINT('',#39140);
#12292=VERTEX_POINT('',#39142);
#12293=VERTEX_POINT('',#39144);
#12294=VERTEX_POINT('',#39146);
#12295=VERTEX_POINT('',#39148);
#12296=VERTEX_POINT('',#39150);
#12297=VERTEX_POINT('',#39152);
#12298=VERTEX_POINT('',#39154);
#12299=VERTEX_POINT('',#39156);
#12300=VERTEX_POINT('',#39158);
#12301=VERTEX_POINT('',#39160);
#12302=VERTEX_POINT('',#39162);
#12303=VERTEX_POINT('',#39165);
#12304=VERTEX_POINT('',#39167);
#12305=VERTEX_POINT('',#39169);
#12306=VERTEX_POINT('',#39171);
#12307=VERTEX_POINT('',#39173);
#12308=VERTEX_POINT('',#39175);
#12309=VERTEX_POINT('',#39177);
#12310=VERTEX_POINT('',#39179);
#12311=VERTEX_POINT('',#39181);
#12312=VERTEX_POINT('',#39183);
#12313=VERTEX_POINT('',#39185);
#12314=VERTEX_POINT('',#39187);
#12315=VERTEX_POINT('',#39189);
#12316=VERTEX_POINT('',#39191);
#12317=VERTEX_POINT('',#39193);
#12318=VERTEX_POINT('',#39195);
#12319=VERTEX_POINT('',#39197);
#12320=VERTEX_POINT('',#39199);
#12321=VERTEX_POINT('',#39202);
#12322=VERTEX_POINT('',#39204);
#12323=VERTEX_POINT('',#39206);
#12324=VERTEX_POINT('',#39208);
#12325=VERTEX_POINT('',#39210);
#12326=VERTEX_POINT('',#39212);
#12327=VERTEX_POINT('',#39214);
#12328=VERTEX_POINT('',#39216);
#12329=VERTEX_POINT('',#39218);
#12330=VERTEX_POINT('',#39220);
#12331=VERTEX_POINT('',#39222);
#12332=VERTEX_POINT('',#39224);
#12333=VERTEX_POINT('',#39226);
#12334=VERTEX_POINT('',#39228);
#12335=VERTEX_POINT('',#39230);
#12336=VERTEX_POINT('',#39232);
#12337=VERTEX_POINT('',#39234);
#12338=VERTEX_POINT('',#39236);
#12339=VERTEX_POINT('',#39239);
#12340=VERTEX_POINT('',#39241);
#12341=VERTEX_POINT('',#39243);
#12342=VERTEX_POINT('',#39245);
#12343=VERTEX_POINT('',#39247);
#12344=VERTEX_POINT('',#39249);
#12345=VERTEX_POINT('',#39251);
#12346=VERTEX_POINT('',#39253);
#12347=VERTEX_POINT('',#39255);
#12348=VERTEX_POINT('',#39257);
#12349=VERTEX_POINT('',#39259);
#12350=VERTEX_POINT('',#39261);
#12351=VERTEX_POINT('',#39263);
#12352=VERTEX_POINT('',#39265);
#12353=VERTEX_POINT('',#39267);
#12354=VERTEX_POINT('',#39269);
#12355=VERTEX_POINT('',#39271);
#12356=VERTEX_POINT('',#39273);
#12357=VERTEX_POINT('',#39276);
#12358=VERTEX_POINT('',#39278);
#12359=VERTEX_POINT('',#39280);
#12360=VERTEX_POINT('',#39282);
#12361=VERTEX_POINT('',#39284);
#12362=VERTEX_POINT('',#39286);
#12363=VERTEX_POINT('',#39288);
#12364=VERTEX_POINT('',#39290);
#12365=VERTEX_POINT('',#39292);
#12366=VERTEX_POINT('',#39294);
#12367=VERTEX_POINT('',#39296);
#12368=VERTEX_POINT('',#39298);
#12369=VERTEX_POINT('',#39300);
#12370=VERTEX_POINT('',#39302);
#12371=VERTEX_POINT('',#39304);
#12372=VERTEX_POINT('',#39306);
#12373=VERTEX_POINT('',#39308);
#12374=VERTEX_POINT('',#39310);
#12375=VERTEX_POINT('',#39313);
#12376=VERTEX_POINT('',#39315);
#12377=VERTEX_POINT('',#39317);
#12378=VERTEX_POINT('',#39319);
#12379=VERTEX_POINT('',#39321);
#12380=VERTEX_POINT('',#39323);
#12381=VERTEX_POINT('',#39325);
#12382=VERTEX_POINT('',#39327);
#12383=VERTEX_POINT('',#39329);
#12384=VERTEX_POINT('',#39331);
#12385=VERTEX_POINT('',#39333);
#12386=VERTEX_POINT('',#39335);
#12387=VERTEX_POINT('',#39337);
#12388=VERTEX_POINT('',#39339);
#12389=VERTEX_POINT('',#39341);
#12390=VERTEX_POINT('',#39343);
#12391=VERTEX_POINT('',#39345);
#12392=VERTEX_POINT('',#39347);
#12393=VERTEX_POINT('',#39350);
#12394=VERTEX_POINT('',#39352);
#12395=VERTEX_POINT('',#39354);
#12396=VERTEX_POINT('',#39356);
#12397=VERTEX_POINT('',#39358);
#12398=VERTEX_POINT('',#39360);
#12399=VERTEX_POINT('',#39362);
#12400=VERTEX_POINT('',#39364);
#12401=VERTEX_POINT('',#39366);
#12402=VERTEX_POINT('',#39368);
#12403=VERTEX_POINT('',#39370);
#12404=VERTEX_POINT('',#39372);
#12405=VERTEX_POINT('',#39374);
#12406=VERTEX_POINT('',#39376);
#12407=VERTEX_POINT('',#39378);
#12408=VERTEX_POINT('',#39380);
#12409=VERTEX_POINT('',#39382);
#12410=VERTEX_POINT('',#39384);
#12411=VERTEX_POINT('',#39387);
#12412=VERTEX_POINT('',#39389);
#12413=VERTEX_POINT('',#39391);
#12414=VERTEX_POINT('',#39393);
#12415=VERTEX_POINT('',#39395);
#12416=VERTEX_POINT('',#39397);
#12417=VERTEX_POINT('',#39399);
#12418=VERTEX_POINT('',#39401);
#12419=VERTEX_POINT('',#39403);
#12420=VERTEX_POINT('',#39405);
#12421=VERTEX_POINT('',#39407);
#12422=VERTEX_POINT('',#39409);
#12423=VERTEX_POINT('',#39411);
#12424=VERTEX_POINT('',#39413);
#12425=VERTEX_POINT('',#39415);
#12426=VERTEX_POINT('',#39417);
#12427=VERTEX_POINT('',#39419);
#12428=VERTEX_POINT('',#39421);
#12429=VERTEX_POINT('',#39424);
#12430=VERTEX_POINT('',#39426);
#12431=VERTEX_POINT('',#39428);
#12432=VERTEX_POINT('',#39430);
#12433=VERTEX_POINT('',#39432);
#12434=VERTEX_POINT('',#39434);
#12435=VERTEX_POINT('',#39436);
#12436=VERTEX_POINT('',#39438);
#12437=VERTEX_POINT('',#39440);
#12438=VERTEX_POINT('',#39442);
#12439=VERTEX_POINT('',#39444);
#12440=VERTEX_POINT('',#39446);
#12441=VERTEX_POINT('',#39448);
#12442=VERTEX_POINT('',#39450);
#12443=VERTEX_POINT('',#39452);
#12444=VERTEX_POINT('',#39454);
#12445=VERTEX_POINT('',#39456);
#12446=VERTEX_POINT('',#39458);
#12447=VERTEX_POINT('',#39461);
#12448=VERTEX_POINT('',#39463);
#12449=VERTEX_POINT('',#39465);
#12450=VERTEX_POINT('',#39467);
#12451=VERTEX_POINT('',#39469);
#12452=VERTEX_POINT('',#39471);
#12453=VERTEX_POINT('',#39473);
#12454=VERTEX_POINT('',#39475);
#12455=VERTEX_POINT('',#39477);
#12456=VERTEX_POINT('',#39479);
#12457=VERTEX_POINT('',#39481);
#12458=VERTEX_POINT('',#39483);
#12459=VERTEX_POINT('',#39485);
#12460=VERTEX_POINT('',#39487);
#12461=VERTEX_POINT('',#39489);
#12462=VERTEX_POINT('',#39491);
#12463=VERTEX_POINT('',#39493);
#12464=VERTEX_POINT('',#39495);
#12465=VERTEX_POINT('',#39498);
#12466=VERTEX_POINT('',#39500);
#12467=VERTEX_POINT('',#39502);
#12468=VERTEX_POINT('',#39504);
#12469=VERTEX_POINT('',#39506);
#12470=VERTEX_POINT('',#39508);
#12471=VERTEX_POINT('',#39510);
#12472=VERTEX_POINT('',#39512);
#12473=VERTEX_POINT('',#39514);
#12474=VERTEX_POINT('',#39516);
#12475=VERTEX_POINT('',#39518);
#12476=VERTEX_POINT('',#39520);
#12477=VERTEX_POINT('',#39522);
#12478=VERTEX_POINT('',#39524);
#12479=VERTEX_POINT('',#39526);
#12480=VERTEX_POINT('',#39528);
#12481=VERTEX_POINT('',#39530);
#12482=VERTEX_POINT('',#39532);
#12483=VERTEX_POINT('',#39535);
#12484=VERTEX_POINT('',#39538);
#12485=VERTEX_POINT('',#39543);
#12486=VERTEX_POINT('',#39545);
#12487=VERTEX_POINT('',#39549);
#12488=VERTEX_POINT('',#39554);
#12489=VERTEX_POINT('',#39556);
#12490=VERTEX_POINT('',#39560);
#12491=VERTEX_POINT('',#39565);
#12492=VERTEX_POINT('',#39567);
#12493=VERTEX_POINT('',#39571);
#12494=VERTEX_POINT('',#39576);
#12495=VERTEX_POINT('',#39578);
#12496=VERTEX_POINT('',#39582);
#12497=VERTEX_POINT('',#39587);
#12498=VERTEX_POINT('',#39589);
#12499=VERTEX_POINT('',#39593);
#12500=VERTEX_POINT('',#39598);
#12501=VERTEX_POINT('',#39600);
#12502=VERTEX_POINT('',#39604);
#12503=VERTEX_POINT('',#39609);
#12504=VERTEX_POINT('',#39611);
#12505=VERTEX_POINT('',#39615);
#12506=VERTEX_POINT('',#39620);
#12507=VERTEX_POINT('',#39622);
#12508=VERTEX_POINT('',#39626);
#12509=VERTEX_POINT('',#39631);
#12510=VERTEX_POINT('',#39633);
#12511=VERTEX_POINT('',#39637);
#12512=VERTEX_POINT('',#39642);
#12513=VERTEX_POINT('',#39644);
#12514=VERTEX_POINT('',#39648);
#12515=VERTEX_POINT('',#39653);
#12516=VERTEX_POINT('',#39655);
#12517=VERTEX_POINT('',#39659);
#12518=VERTEX_POINT('',#40120);
#12519=VERTEX_POINT('',#40125);
#12520=VERTEX_POINT('',#40131);
#12521=VERTEX_POINT('',#40132);
#12522=VERTEX_POINT('',#40134);
#12523=VERTEX_POINT('',#40136);
#12524=VERTEX_POINT('',#40140);
#12525=VERTEX_POINT('',#40142);
#12526=VERTEX_POINT('',#40146);
#12527=VERTEX_POINT('',#40148);
#12528=VERTEX_POINT('',#40156);
#12529=VERTEX_POINT('',#40157);
#12530=VERTEX_POINT('',#40159);
#12531=VERTEX_POINT('',#40161);
#12532=VERTEX_POINT('',#40165);
#12533=VERTEX_POINT('',#40167);
#12534=VERTEX_POINT('',#40171);
#12535=VERTEX_POINT('',#40173);
#12536=VERTEX_POINT('',#40181);
#12537=VERTEX_POINT('',#40183);
#12538=VERTEX_POINT('',#40187);
#12539=VERTEX_POINT('',#40189);
#12540=VERTEX_POINT('',#40193);
#12541=VERTEX_POINT('',#40194);
#12542=VERTEX_POINT('',#40196);
#12543=VERTEX_POINT('',#40198);
#12544=VERTEX_POINT('',#40208);
#12545=VERTEX_POINT('',#40209);
#12546=VERTEX_POINT('',#40212);
#12547=VERTEX_POINT('',#40216);
#12548=VERTEX_POINT('',#40219);
#12549=VERTEX_POINT('',#40223);
#12550=VERTEX_POINT('',#40227);
#12551=VERTEX_POINT('',#40230);
#12552=VERTEX_POINT('',#40234);
#12553=VERTEX_POINT('',#40237);
#12554=VERTEX_POINT('',#40241);
#12555=VERTEX_POINT('',#40247);
#12556=VERTEX_POINT('',#40248);
#12557=VERTEX_POINT('',#40250);
#12558=VERTEX_POINT('',#40252);
#12559=VERTEX_POINT('',#40259);
#12560=VERTEX_POINT('',#40261);
#12561=VERTEX_POINT('',#40268);
#12562=VERTEX_POINT('',#40270);
#12563=VERTEX_POINT('',#40274);
#12564=VERTEX_POINT('',#40276);
#12565=VERTEX_POINT('',#40280);
#12566=VERTEX_POINT('',#40284);
#12567=VERTEX_POINT('',#40288);
#12568=VERTEX_POINT('',#40290);
#12569=VERTEX_POINT('',#40297);
#12570=VERTEX_POINT('',#40304);
#12571=VERTEX_POINT('',#40309);
#12572=VERTEX_POINT('',#40311);
#12573=VERTEX_POINT('',#40316);
#12574=VERTEX_POINT('',#40320);
#12575=VERTEX_POINT('',#40324);
#12576=VERTEX_POINT('',#40328);
#12577=VERTEX_POINT('',#40331);
#12578=VERTEX_POINT('',#40335);
#12579=VERTEX_POINT('',#40342);
#12580=VERTEX_POINT('',#40343);
#12581=VERTEX_POINT('',#40345);
#12582=VERTEX_POINT('',#40347);
#12583=VERTEX_POINT('',#40349);
#12584=VERTEX_POINT('',#40351);
#12585=VERTEX_POINT('',#40355);
#12586=VERTEX_POINT('',#40357);
#12587=VERTEX_POINT('',#40361);
#12588=VERTEX_POINT('',#40363);
#12589=VERTEX_POINT('',#40365);
#12590=VERTEX_POINT('',#40369);
#12591=VERTEX_POINT('',#40371);
#12592=VERTEX_POINT('',#40373);
#12593=VERTEX_POINT('',#40377);
#12594=VERTEX_POINT('',#40379);
#12595=VERTEX_POINT('',#40381);
#12596=VERTEX_POINT('',#40383);
#12597=VERTEX_POINT('',#40387);
#12598=VERTEX_POINT('',#40389);
#12599=VERTEX_POINT('',#40393);
#12600=VERTEX_POINT('',#40395);
#12601=VERTEX_POINT('',#40397);
#12602=VERTEX_POINT('',#40401);
#12603=VERTEX_POINT('',#40406);
#12604=VERTEX_POINT('',#40410);
#12605=VERTEX_POINT('',#40412);
#12606=VERTEX_POINT('',#40414);
#12607=VERTEX_POINT('',#40418);
#12608=VERTEX_POINT('',#40423);
#12609=VERTEX_POINT('',#40427);
#12610=VERTEX_POINT('',#40429);
#12611=VERTEX_POINT('',#40441);
#12612=VERTEX_POINT('',#40442);
#12613=VERTEX_POINT('',#40445);
#12614=VERTEX_POINT('',#40447);
#12615=VERTEX_POINT('',#40451);
#12616=VERTEX_POINT('',#40453);
#12617=VERTEX_POINT('',#40457);
#12618=VERTEX_POINT('',#40459);
#12619=VERTEX_POINT('',#40466);
#12620=VERTEX_POINT('',#40467);
#12621=VERTEX_POINT('',#40469);
#12622=VERTEX_POINT('',#40473);
#12623=VERTEX_POINT('',#40474);
#12624=VERTEX_POINT('',#40476);
#12625=VERTEX_POINT('',#40480);
#12626=VERTEX_POINT('',#40481);
#12627=VERTEX_POINT('',#40483);
#12628=VERTEX_POINT('',#40487);
#12629=VERTEX_POINT('',#40488);
#12630=VERTEX_POINT('',#40490);
#12631=VERTEX_POINT('',#40497);
#12632=VERTEX_POINT('',#40498);
#12633=VERTEX_POINT('',#40500);
#12634=VERTEX_POINT('',#40504);
#12635=VERTEX_POINT('',#40505);
#12636=VERTEX_POINT('',#40507);
#12637=VERTEX_POINT('',#40517);
#12638=VERTEX_POINT('',#40518);
#12639=VERTEX_POINT('',#40528);
#12640=VERTEX_POINT('',#40529);
#12641=VERTEX_POINT('',#40536);
#12642=VERTEX_POINT('',#40537);
#12643=VERTEX_POINT('',#40547);
#12644=VERTEX_POINT('',#40548);
#12645=VERTEX_POINT('',#40555);
#12646=VERTEX_POINT('',#40556);
#12647=VERTEX_POINT('',#40566);
#12648=VERTEX_POINT('',#40567);
#12649=VERTEX_POINT('',#40578);
#12650=VERTEX_POINT('',#40590);
#12651=VERTEX_POINT('',#40593);
#12652=VERTEX_POINT('',#40594);
#12653=VERTEX_POINT('',#40596);
#12654=VERTEX_POINT('',#40598);
#12655=VERTEX_POINT('',#40602);
#12656=VERTEX_POINT('',#40604);
#12657=VERTEX_POINT('',#40608);
#12658=VERTEX_POINT('',#40609);
#12659=VERTEX_POINT('',#40611);
#12660=VERTEX_POINT('',#40613);
#12661=VERTEX_POINT('',#40617);
#12662=VERTEX_POINT('',#40619);
#12663=VERTEX_POINT('',#40629);
#12664=VERTEX_POINT('',#40631);
#12665=VERTEX_POINT('',#40635);
#12666=VERTEX_POINT('',#40639);
#12667=VERTEX_POINT('',#40643);
#12668=VERTEX_POINT('',#40646);
#12669=VERTEX_POINT('',#40650);
#12670=VERTEX_POINT('',#40671);
#12671=VERTEX_POINT('',#40674);
#12672=VERTEX_POINT('',#40678);
#12673=VERTEX_POINT('',#40682);
#12674=VERTEX_POINT('',#40688);
#12675=VERTEX_POINT('',#40690);
#12676=VERTEX_POINT('',#40694);
#12677=VERTEX_POINT('',#40697);
#12678=VERTEX_POINT('',#40700);
#12679=VERTEX_POINT('',#40704);
#12680=VERTEX_POINT('',#40706);
#12681=VERTEX_POINT('',#40710);
#12682=VERTEX_POINT('',#40713);
#12683=VERTEX_POINT('',#40717);
#12684=VERTEX_POINT('',#40720);
#12685=VERTEX_POINT('',#40725);
#12686=VERTEX_POINT('',#40731);
#12687=VERTEX_POINT('',#40732);
#12688=VERTEX_POINT('',#40734);
#12689=VERTEX_POINT('',#40751);
#12690=VERTEX_POINT('',#40764);
#12691=VERTEX_POINT('',#40765);
#12692=VERTEX_POINT('',#40848);
#12693=VERTEX_POINT('',#40849);
#12694=VERTEX_POINT('',#40938);
#12695=VERTEX_POINT('',#40939);
#12696=VERTEX_POINT('',#41028);
#12697=VERTEX_POINT('',#41029);
#12698=VERTEX_POINT('',#41112);
#12699=VERTEX_POINT('',#41113);
#12700=VERTEX_POINT('',#41202);
#12701=VERTEX_POINT('',#41203);
#12702=VERTEX_POINT('',#41292);
#12703=VERTEX_POINT('',#41293);
#12704=VERTEX_POINT('',#41376);
#12705=VERTEX_POINT('',#41377);
#12706=VERTEX_POINT('',#41466);
#12707=VERTEX_POINT('',#41467);
#12708=VERTEX_POINT('',#41544);
#12709=VERTEX_POINT('',#41545);
#12710=VERTEX_POINT('',#41592);
#12711=VERTEX_POINT('',#41593);
#12712=VERTEX_POINT('',#41646);
#12713=VERTEX_POINT('',#41647);
#12714=VERTEX_POINT('',#41730);
#12715=VERTEX_POINT('',#41731);
#12716=VERTEX_POINT('',#41814);
#12717=VERTEX_POINT('',#41815);
#12718=VERTEX_POINT('',#41904);
#12719=VERTEX_POINT('',#41905);
#12720=VERTEX_POINT('',#41994);
#12721=VERTEX_POINT('',#41995);
#12722=VERTEX_POINT('',#42078);
#12723=VERTEX_POINT('',#42079);
#12724=VERTEX_POINT('',#42168);
#12725=VERTEX_POINT('',#42169);
#12726=VERTEX_POINT('',#42258);
#12727=VERTEX_POINT('',#42259);
#12728=VERTEX_POINT('',#42342);
#12729=VERTEX_POINT('',#42343);
#12730=VERTEX_POINT('',#42345);
#12731=VERTEX_POINT('',#42428);
#12732=VERTEX_POINT('',#42429);
#12733=VERTEX_POINT('',#42431);
#12734=VERTEX_POINT('',#42443);
#12735=VERTEX_POINT('',#42454);
#12736=VERTEX_POINT('',#42455);
#12737=VERTEX_POINT('',#42491);
#12738=VERTEX_POINT('',#42492);
#12739=VERTEX_POINT('',#42528);
#12740=VERTEX_POINT('',#42529);
#12741=VERTEX_POINT('',#42566);
#12742=VERTEX_POINT('',#42567);
#12743=VERTEX_POINT('',#42603);
#12744=VERTEX_POINT('',#42604);
#12745=VERTEX_POINT('',#42640);
#12746=VERTEX_POINT('',#42641);
#12747=VERTEX_POINT('',#42678);
#12748=VERTEX_POINT('',#42679);
#12749=VERTEX_POINT('',#42715);
#12750=VERTEX_POINT('',#42716);
#12751=VERTEX_POINT('',#42752);
#12752=VERTEX_POINT('',#42753);
#12753=VERTEX_POINT('',#42783);
#12754=VERTEX_POINT('',#42784);
#12755=VERTEX_POINT('',#42807);
#12756=VERTEX_POINT('',#42808);
#12757=VERTEX_POINT('',#42835);
#12758=VERTEX_POINT('',#42836);
#12759=VERTEX_POINT('',#42872);
#12760=VERTEX_POINT('',#42873);
#12761=VERTEX_POINT('',#42909);
#12762=VERTEX_POINT('',#42910);
#12763=VERTEX_POINT('',#42946);
#12764=VERTEX_POINT('',#42947);
#12765=VERTEX_POINT('',#42984);
#12766=VERTEX_POINT('',#42985);
#12767=VERTEX_POINT('',#43021);
#12768=VERTEX_POINT('',#43022);
#12769=VERTEX_POINT('',#43058);
#12770=VERTEX_POINT('',#43059);
#12771=VERTEX_POINT('',#43096);
#12772=VERTEX_POINT('',#43097);
#12773=VERTEX_POINT('',#43236);
#12774=VERTEX_POINT('',#44333);
#12775=VERTEX_POINT('',#44452);
#12776=VERTEX_POINT('',#44455);
#12777=VERTEX_POINT('',#45570);
#12778=VERTEX_POINT('',#45571);
#12779=VERTEX_POINT('',#45573);
#12780=VERTEX_POINT('',#45575);
#12781=VERTEX_POINT('',#45579);
#12782=VERTEX_POINT('',#45583);
#12783=VERTEX_POINT('',#45589);
#12784=VERTEX_POINT('',#45590);
#12785=VERTEX_POINT('',#45592);
#12786=VERTEX_POINT('',#45594);
#12787=VERTEX_POINT('',#45598);
#12788=VERTEX_POINT('',#45602);
#12789=VERTEX_POINT('',#45608);
#12790=VERTEX_POINT('',#45609);
#12791=VERTEX_POINT('',#45611);
#12792=VERTEX_POINT('',#45613);
#12793=VERTEX_POINT('',#45617);
#12794=VERTEX_POINT('',#45621);
#12795=VERTEX_POINT('',#45627);
#12796=VERTEX_POINT('',#45628);
#12797=VERTEX_POINT('',#45630);
#12798=VERTEX_POINT('',#45632);
#12799=VERTEX_POINT('',#45636);
#12800=VERTEX_POINT('',#45640);
#12801=VERTEX_POINT('',#45646);
#12802=VERTEX_POINT('',#45647);
#12803=VERTEX_POINT('',#45649);
#12804=VERTEX_POINT('',#45651);
#12805=VERTEX_POINT('',#45655);
#12806=VERTEX_POINT('',#45659);
#12807=VERTEX_POINT('',#45665);
#12808=VERTEX_POINT('',#45666);
#12809=VERTEX_POINT('',#45668);
#12810=VERTEX_POINT('',#45670);
#12811=VERTEX_POINT('',#45674);
#12812=VERTEX_POINT('',#45678);
#12813=VERTEX_POINT('',#45684);
#12814=VERTEX_POINT('',#45685);
#12815=VERTEX_POINT('',#45687);
#12816=VERTEX_POINT('',#45689);
#12817=VERTEX_POINT('',#45693);
#12818=VERTEX_POINT('',#45697);
#12819=VERTEX_POINT('',#45703);
#12820=VERTEX_POINT('',#45704);
#12821=VERTEX_POINT('',#45706);
#12822=VERTEX_POINT('',#45708);
#12823=VERTEX_POINT('',#45712);
#12824=VERTEX_POINT('',#45716);
#12825=VERTEX_POINT('',#45722);
#12826=VERTEX_POINT('',#45723);
#12827=VERTEX_POINT('',#45725);
#12828=VERTEX_POINT('',#45727);
#12829=VERTEX_POINT('',#45731);
#12830=VERTEX_POINT('',#45735);
#12831=VERTEX_POINT('',#45741);
#12832=VERTEX_POINT('',#45742);
#12833=VERTEX_POINT('',#45744);
#12834=VERTEX_POINT('',#45746);
#12835=VERTEX_POINT('',#45750);
#12836=VERTEX_POINT('',#45754);
#12837=VERTEX_POINT('',#45760);
#12838=VERTEX_POINT('',#45761);
#12839=VERTEX_POINT('',#45763);
#12840=VERTEX_POINT('',#45765);
#12841=VERTEX_POINT('',#45769);
#12842=VERTEX_POINT('',#45773);
#12843=VERTEX_POINT('',#45779);
#12844=VERTEX_POINT('',#45780);
#12845=VERTEX_POINT('',#45782);
#12846=VERTEX_POINT('',#45784);
#12847=VERTEX_POINT('',#45788);
#12848=VERTEX_POINT('',#45792);
#12849=VERTEX_POINT('',#45798);
#12850=VERTEX_POINT('',#45799);
#12851=VERTEX_POINT('',#45801);
#12852=VERTEX_POINT('',#45803);
#12853=VERTEX_POINT('',#45807);
#12854=VERTEX_POINT('',#45811);
#12855=VERTEX_POINT('',#45817);
#12856=VERTEX_POINT('',#45818);
#12857=VERTEX_POINT('',#45820);
#12858=VERTEX_POINT('',#45822);
#12859=VERTEX_POINT('',#45826);
#12860=VERTEX_POINT('',#45830);
#12861=VERTEX_POINT('',#45836);
#12862=VERTEX_POINT('',#45837);
#12863=VERTEX_POINT('',#45839);
#12864=VERTEX_POINT('',#45841);
#12865=VERTEX_POINT('',#45845);
#12866=VERTEX_POINT('',#45849);
#12867=VERTEX_POINT('',#45855);
#12868=VERTEX_POINT('',#45856);
#12869=VERTEX_POINT('',#45858);
#12870=VERTEX_POINT('',#45860);
#12871=VERTEX_POINT('',#45864);
#12872=VERTEX_POINT('',#45868);
#12873=VERTEX_POINT('',#45874);
#12874=VERTEX_POINT('',#45875);
#12875=VERTEX_POINT('',#45877);
#12876=VERTEX_POINT('',#45879);
#12877=VERTEX_POINT('',#45883);
#12878=VERTEX_POINT('',#45887);
#12879=VERTEX_POINT('',#45893);
#12880=VERTEX_POINT('',#45894);
#12881=VERTEX_POINT('',#45896);
#12882=VERTEX_POINT('',#45898);
#12883=VERTEX_POINT('',#45902);
#12884=VERTEX_POINT('',#45904);
#12885=VERTEX_POINT('',#45908);
#12886=VERTEX_POINT('',#45912);
#12887=VERTEX_POINT('',#45916);
#12888=VERTEX_POINT('',#45917);
#12889=VERTEX_POINT('',#45919);
#12890=VERTEX_POINT('',#45921);
#12891=VERTEX_POINT('',#45925);
#12892=VERTEX_POINT('',#45929);
#12893=VERTEX_POINT('',#45935);
#12894=VERTEX_POINT('',#45936);
#12895=VERTEX_POINT('',#45938);
#12896=VERTEX_POINT('',#45940);
#12897=VERTEX_POINT('',#45944);
#12898=VERTEX_POINT('',#45948);
#12899=VERTEX_POINT('',#45954);
#12900=VERTEX_POINT('',#45955);
#12901=VERTEX_POINT('',#45957);
#12902=VERTEX_POINT('',#45959);
#12903=VERTEX_POINT('',#45963);
#12904=VERTEX_POINT('',#45967);
#12905=VERTEX_POINT('',#45973);
#12906=VERTEX_POINT('',#45974);
#12907=VERTEX_POINT('',#45976);
#12908=VERTEX_POINT('',#45978);
#12909=VERTEX_POINT('',#45982);
#12910=VERTEX_POINT('',#45986);
#12911=VERTEX_POINT('',#45992);
#12912=VERTEX_POINT('',#45993);
#12913=VERTEX_POINT('',#45995);
#12914=VERTEX_POINT('',#45997);
#12915=VERTEX_POINT('',#46001);
#12916=VERTEX_POINT('',#46005);
#12917=VERTEX_POINT('',#46011);
#12918=VERTEX_POINT('',#46012);
#12919=VERTEX_POINT('',#46014);
#12920=VERTEX_POINT('',#46016);
#12921=VERTEX_POINT('',#46020);
#12922=VERTEX_POINT('',#46024);
#12923=VERTEX_POINT('',#46030);
#12924=VERTEX_POINT('',#46031);
#12925=VERTEX_POINT('',#46033);
#12926=VERTEX_POINT('',#46035);
#12927=VERTEX_POINT('',#46039);
#12928=VERTEX_POINT('',#46043);
#12929=VERTEX_POINT('',#46049);
#12930=VERTEX_POINT('',#46050);
#12931=VERTEX_POINT('',#46052);
#12932=VERTEX_POINT('',#46054);
#12933=VERTEX_POINT('',#46058);
#12934=VERTEX_POINT('',#46062);
#12935=VERTEX_POINT('',#46068);
#12936=VERTEX_POINT('',#46069);
#12937=VERTEX_POINT('',#46071);
#12938=VERTEX_POINT('',#46073);
#12939=VERTEX_POINT('',#46077);
#12940=VERTEX_POINT('',#46081);
#12941=VERTEX_POINT('',#46087);
#12942=VERTEX_POINT('',#46088);
#12943=VERTEX_POINT('',#46090);
#12944=VERTEX_POINT('',#46092);
#12945=VERTEX_POINT('',#46096);
#12946=VERTEX_POINT('',#46100);
#12947=VERTEX_POINT('',#46106);
#12948=VERTEX_POINT('',#46107);
#12949=VERTEX_POINT('',#46109);
#12950=VERTEX_POINT('',#46111);
#12951=VERTEX_POINT('',#46115);
#12952=VERTEX_POINT('',#46119);
#12953=VERTEX_POINT('',#46125);
#12954=VERTEX_POINT('',#46126);
#12955=VERTEX_POINT('',#46128);
#12956=VERTEX_POINT('',#46130);
#12957=VERTEX_POINT('',#46134);
#12958=VERTEX_POINT('',#46138);
#12959=VERTEX_POINT('',#46144);
#12960=VERTEX_POINT('',#46145);
#12961=VERTEX_POINT('',#46147);
#12962=VERTEX_POINT('',#46149);
#12963=VERTEX_POINT('',#46153);
#12964=VERTEX_POINT('',#46157);
#12965=VERTEX_POINT('',#46163);
#12966=VERTEX_POINT('',#46164);
#12967=VERTEX_POINT('',#46166);
#12968=VERTEX_POINT('',#46168);
#12969=VERTEX_POINT('',#46172);
#12970=VERTEX_POINT('',#46176);
#12971=VERTEX_POINT('',#46182);
#12972=VERTEX_POINT('',#46183);
#12973=VERTEX_POINT('',#46185);
#12974=VERTEX_POINT('',#46187);
#12975=VERTEX_POINT('',#46191);
#12976=VERTEX_POINT('',#46195);
#12977=VERTEX_POINT('',#46201);
#12978=VERTEX_POINT('',#46202);
#12979=VERTEX_POINT('',#46204);
#12980=VERTEX_POINT('',#46206);
#12981=VERTEX_POINT('',#46210);
#12982=VERTEX_POINT('',#46214);
#12983=VERTEX_POINT('',#46220);
#12984=VERTEX_POINT('',#46221);
#12985=VERTEX_POINT('',#46223);
#12986=VERTEX_POINT('',#46225);
#12987=VERTEX_POINT('',#46229);
#12988=VERTEX_POINT('',#46233);
#12989=VERTEX_POINT('',#46239);
#12990=VERTEX_POINT('',#46240);
#12991=VERTEX_POINT('',#46242);
#12992=VERTEX_POINT('',#46244);
#12993=VERTEX_POINT('',#46248);
#12994=VERTEX_POINT('',#46252);
#12995=VERTEX_POINT('',#46258);
#12996=VERTEX_POINT('',#46259);
#12997=VERTEX_POINT('',#46261);
#12998=VERTEX_POINT('',#46263);
#12999=VERTEX_POINT('',#46267);
#13000=VERTEX_POINT('',#46269);
#13001=VERTEX_POINT('',#46273);
#13002=VERTEX_POINT('',#46275);
#13003=VERTEX_POINT('',#46279);
#13004=VERTEX_POINT('',#46281);
#13005=VERTEX_POINT('',#46285);
#13006=VERTEX_POINT('',#46287);
#13007=VERTEX_POINT('',#46295);
#13008=VERTEX_POINT('',#46302);
#13009=VERTEX_POINT('',#46306);
#13010=VERTEX_POINT('',#46310);
#13011=VERTEX_POINT('',#46313);
#13012=VERTEX_POINT('',#46318);
#13013=VERTEX_POINT('',#46324);
#13014=VERTEX_POINT('',#46327);
#13015=VERTEX_POINT('',#46331);
#13016=VERTEX_POINT('',#46335);
#13017=EDGE_CURVE('',#10734,#10734,#10272,.T.);
#13018=EDGE_CURVE('',#10734,#10735,#4534,.T.);
#13019=EDGE_CURVE('',#10735,#10735,#10273,.T.);
#13020=EDGE_CURVE('',#10736,#10736,#10274,.T.);
#13021=EDGE_CURVE('',#10735,#10737,#4535,.T.);
#13022=EDGE_CURVE('',#10737,#10737,#10275,.T.);
#13023=EDGE_CURVE('',#10738,#10738,#10276,.T.);
#13024=EDGE_CURVE('',#10738,#10739,#4536,.T.);
#13025=EDGE_CURVE('',#10739,#10739,#10277,.T.);
#13026=EDGE_CURVE('',#10740,#10740,#10278,.T.);
#13027=EDGE_CURVE('',#10739,#10741,#4537,.T.);
#13028=EDGE_CURVE('',#10741,#10741,#10279,.T.);
#13029=EDGE_CURVE('',#10742,#10742,#10280,.T.);
#13030=EDGE_CURVE('',#10742,#10743,#4538,.T.);
#13031=EDGE_CURVE('',#10743,#10744,#10281,.T.);
#13032=EDGE_CURVE('',#10744,#10743,#10282,.T.);
#13033=EDGE_CURVE('',#10744,#10745,#4539,.T.);
#13034=EDGE_CURVE('',#10745,#10745,#10283,.T.);
#13035=EDGE_CURVE('',#10746,#10746,#10284,.T.);
#13036=EDGE_CURVE('',#10747,#10747,#10285,.T.);
#13037=EDGE_CURVE('',#10747,#10745,#4540,.T.);
#13038=EDGE_CURVE('',#10748,#10749,#4541,.T.);
#13039=EDGE_CURVE('',#10750,#10748,#10286,.T.);
#13040=EDGE_CURVE('',#10751,#10750,#4542,.T.);
#13041=EDGE_CURVE('',#10749,#10751,#10287,.T.);
#13042=EDGE_CURVE('',#10752,#10753,#235,.T.);
#13043=EDGE_CURVE('',#10754,#10753,#236,.T.);
#13044=EDGE_CURVE('',#10754,#10755,#237,.T.);
#13045=EDGE_CURVE('',#10755,#10752,#4543,.T.);
#13046=EDGE_CURVE('',#10753,#10756,#238,.T.);
#13047=EDGE_CURVE('',#10756,#10757,#4544,.T.);
#13048=EDGE_CURVE('',#10757,#10754,#239,.T.);
#13049=EDGE_CURVE('',#10758,#10759,#4545,.F.);
#13050=EDGE_CURVE('',#10759,#10757,#4546,.T.);
#13051=EDGE_CURVE('',#10756,#10758,#4547,.T.);
#13052=EDGE_CURVE('',#10760,#10761,#4548,.T.);
#13053=EDGE_CURVE('',#10762,#10760,#10288,.T.);
#13054=EDGE_CURVE('',#10763,#10762,#4549,.T.);
#13055=EDGE_CURVE('',#10764,#10763,#10289,.T.);
#13056=EDGE_CURVE('',#10765,#10764,#4550,.T.);
#13057=EDGE_CURVE('',#10766,#10765,#10290,.T.);
#13058=EDGE_CURVE('',#10767,#10766,#4551,.T.);
#13059=EDGE_CURVE('',#10768,#10767,#10291,.T.);
#13060=EDGE_CURVE('',#10769,#10768,#4552,.T.);
#13061=EDGE_CURVE('',#10761,#10769,#10292,.T.);
#13062=EDGE_CURVE('',#10770,#10770,#10293,.T.);
#13063=EDGE_CURVE('',#10771,#10755,#4553,.T.);
#13064=EDGE_CURVE('',#10772,#10771,#4554,.T.);
#13065=EDGE_CURVE('',#10773,#10772,#4555,.T.);
#13066=EDGE_CURVE('',#10774,#10773,#10294,.T.);
#13067=EDGE_CURVE('',#10775,#10774,#4556,.T.);
#13068=EDGE_CURVE('',#10776,#10775,#4557,.T.);
#13069=EDGE_CURVE('',#10777,#10776,#4558,.T.);
#13070=EDGE_CURVE('',#10778,#10777,#10295,.T.);
#13071=EDGE_CURVE('',#10779,#10778,#10296,.T.);
#13072=EDGE_CURVE('',#10780,#10779,#4559,.T.);
#13073=EDGE_CURVE('',#10781,#10780,#10297,.T.);
#13074=EDGE_CURVE('',#10782,#10781,#4560,.T.);
#13075=EDGE_CURVE('',#10783,#10782,#10298,.T.);
#13076=EDGE_CURVE('',#10784,#10783,#4561,.T.);
#13077=EDGE_CURVE('',#10785,#10784,#10299,.T.);
#13078=EDGE_CURVE('',#10786,#10785,#10300,.T.);
#13079=EDGE_CURVE('',#10787,#10786,#4562,.T.);
#13080=EDGE_CURVE('',#10788,#10787,#4563,.T.);
#13081=EDGE_CURVE('',#10789,#10788,#4564,.T.);
#13082=EDGE_CURVE('',#10790,#10789,#4565,.T.);
#13083=EDGE_CURVE('',#10791,#10790,#4566,.T.);
#13084=EDGE_CURVE('',#10792,#10791,#10301,.T.);
#13085=EDGE_CURVE('',#10752,#10792,#4567,.T.);
#13086=EDGE_CURVE('',#10793,#10794,#10302,.T.);
#13087=EDGE_CURVE('',#10795,#10793,#4568,.T.);
#13088=EDGE_CURVE('',#10796,#10795,#10303,.T.);
#13089=EDGE_CURVE('',#10797,#10796,#10304,.T.);
#13090=EDGE_CURVE('',#10794,#10797,#4569,.T.);
#13091=EDGE_CURVE('',#10798,#10799,#10305,.T.);
#13092=EDGE_CURVE('',#10798,#10800,#10306,.T.);
#13093=EDGE_CURVE('',#10800,#10801,#10307,.T.);
#13094=EDGE_CURVE('',#10802,#10801,#10308,.T.);
#13095=EDGE_CURVE('',#10802,#10799,#10309,.T.);
#13096=EDGE_CURVE('',#10803,#10804,#10310,.T.);
#13097=EDGE_CURVE('',#10805,#10803,#4570,.T.);
#13098=EDGE_CURVE('',#10806,#10805,#10311,.T.);
#13099=EDGE_CURVE('',#10807,#10806,#10312,.T.);
#13100=EDGE_CURVE('',#10804,#10807,#4571,.T.);
#13101=EDGE_CURVE('',#10808,#10808,#10313,.T.);
#13102=EDGE_CURVE('',#10757,#10809,#4572,.T.);
#13103=EDGE_CURVE('',#10810,#10809,#240,.T.);
#13104=EDGE_CURVE('',#10771,#10810,#241,.T.);
#13105=EDGE_CURVE('',#10811,#10759,#4573,.T.);
#13106=EDGE_CURVE('',#10809,#10811,#4574,.T.);
#13107=EDGE_CURVE('',#10812,#10810,#242,.T.);
#13108=EDGE_CURVE('',#10812,#10772,#243,.T.);
#13109=EDGE_CURVE('',#10809,#10813,#4575,.T.);
#13110=EDGE_CURVE('',#10813,#10812,#244,.T.);
#13111=EDGE_CURVE('',#10811,#10814,#4576,.F.);
#13112=EDGE_CURVE('',#10814,#10813,#4577,.T.);
#13113=EDGE_CURVE('',#10813,#10815,#4578,.T.);
#13114=EDGE_CURVE('',#10773,#10815,#245,.F.);
#13115=EDGE_CURVE('',#10816,#10814,#4579,.T.);
#13116=EDGE_CURVE('',#10815,#10816,#4580,.T.);
#13117=EDGE_CURVE('',#10740,#10817,#4581,.T.);
#13118=EDGE_CURVE('',#10817,#10817,#10314,.T.);
#13119=EDGE_CURVE('',#10818,#10818,#10315,.T.);
#13120=EDGE_CURVE('',#10818,#10817,#4582,.T.);
#13121=EDGE_CURVE('',#10736,#10819,#4583,.T.);
#13122=EDGE_CURVE('',#10819,#10819,#10316,.T.);
#13123=EDGE_CURVE('',#10820,#10820,#10317,.T.);
#13124=EDGE_CURVE('',#10820,#10819,#4584,.T.);
#13125=EDGE_CURVE('',#10821,#10822,#246,.F.);
#13126=EDGE_CURVE('',#10822,#10823,#4585,.T.);
#13127=EDGE_CURVE('',#10823,#10824,#247,.F.);
#13128=EDGE_CURVE('',#10824,#10821,#4586,.T.);
#13129=EDGE_CURVE('',#10825,#10825,#10318,.T.);
#13130=EDGE_CURVE('',#10825,#10826,#4587,.T.);
#13131=EDGE_CURVE('',#10826,#10827,#10319,.T.);
#13132=EDGE_CURVE('',#10823,#10827,#248,.F.);
#13133=EDGE_CURVE('',#10828,#10822,#10320,.T.);
#13134=EDGE_CURVE('',#10829,#10828,#4588,.T.);
#13135=EDGE_CURVE('',#10830,#10829,#249,.F.);
#13136=EDGE_CURVE('',#10830,#10826,#10321,.T.);
#13137=EDGE_CURVE('',#10831,#10832,#250,.F.);
#13138=EDGE_CURVE('',#10832,#10833,#4589,.T.);
#13139=EDGE_CURVE('',#10833,#10834,#251,.F.);
#13140=EDGE_CURVE('',#10834,#10831,#4590,.T.);
#13141=EDGE_CURVE('',#10835,#10835,#10322,.T.);
#13142=EDGE_CURVE('',#10835,#10836,#4591,.T.);
#13143=EDGE_CURVE('',#10833,#10836,#10323,.T.);
#13144=EDGE_CURVE('',#10837,#10832,#252,.F.);
#13145=EDGE_CURVE('',#10837,#10838,#10324,.T.);
#13146=EDGE_CURVE('',#10839,#10838,#253,.F.);
#13147=EDGE_CURVE('',#10840,#10839,#4592,.T.);
#13148=EDGE_CURVE('',#10836,#10840,#10325,.T.);
#13149=EDGE_CURVE('',#10841,#10840,#254,.F.);
#13150=EDGE_CURVE('',#10839,#10842,#255,.F.);
#13151=EDGE_CURVE('',#10842,#10841,#4593,.T.);
#13152=EDGE_CURVE('',#10843,#10829,#256,.F.);
#13153=EDGE_CURVE('',#10828,#10844,#257,.F.);
#13154=EDGE_CURVE('',#10844,#10843,#4594,.T.);
#13155=EDGE_CURVE('',#10845,#10845,#10326,.T.);
#13156=EDGE_CURVE('',#10845,#10820,#4595,.T.);
#13157=EDGE_CURVE('',#10846,#10847,#10327,.T.);
#13158=EDGE_CURVE('',#10848,#10846,#4596,.T.);
#13159=EDGE_CURVE('',#10849,#10848,#10328,.T.);
#13160=EDGE_CURVE('',#10850,#10849,#4597,.T.);
#13161=EDGE_CURVE('',#10851,#10850,#10329,.T.);
#13162=EDGE_CURVE('',#10852,#10851,#4598,.T.);
#13163=EDGE_CURVE('',#10853,#10852,#10330,.T.);
#13164=EDGE_CURVE('',#10847,#10853,#4599,.T.);
#13165=EDGE_CURVE('',#10854,#10854,#10331,.T.);
#13166=EDGE_CURVE('',#10855,#10855,#10332,.T.);
#13167=EDGE_CURVE('',#10856,#10856,#10333,.T.);
#13168=EDGE_CURVE('',#10857,#10858,#4600,.T.);
#13169=EDGE_CURVE('',#10859,#10857,#10334,.T.);
#13170=EDGE_CURVE('',#10860,#10859,#4601,.T.);
#13171=EDGE_CURVE('',#10858,#10860,#10335,.T.);
#13172=EDGE_CURVE('',#10861,#10861,#10336,.T.);
#13173=EDGE_CURVE('',#10862,#10862,#10337,.T.);
#13174=EDGE_CURVE('',#10863,#10863,#10338,.T.);
#13175=EDGE_CURVE('',#10864,#10864,#10339,.T.);
#13176=EDGE_CURVE('',#10854,#10835,#4602,.T.);
#13177=EDGE_CURVE('',#10864,#10825,#4603,.T.);
#13178=EDGE_CURVE('',#10855,#10818,#4604,.T.);
#13179=EDGE_CURVE('',#10863,#10865,#4605,.T.);
#13180=EDGE_CURVE('',#10865,#10865,#10340,.T.);
#13181=EDGE_CURVE('',#10866,#10866,#10341,.T.);
#13182=EDGE_CURVE('',#10866,#10865,#4606,.T.);
#13183=EDGE_CURVE('',#10856,#10867,#4607,.T.);
#13184=EDGE_CURVE('',#10867,#10867,#10342,.T.);
#13185=EDGE_CURVE('',#10868,#10868,#10343,.T.);
#13186=EDGE_CURVE('',#10868,#10867,#4608,.T.);
#13187=EDGE_CURVE('',#10787,#10869,#258,.T.);
#13188=EDGE_CURVE('',#10870,#10869,#259,.T.);
#13189=EDGE_CURVE('',#10870,#10788,#260,.T.);
#13190=EDGE_CURVE('',#10869,#10871,#261,.T.);
#13191=EDGE_CURVE('',#10871,#10872,#4609,.T.);
#13192=EDGE_CURVE('',#10872,#10870,#262,.T.);
#13193=EDGE_CURVE('',#10873,#10874,#4610,.F.);
#13194=EDGE_CURVE('',#10874,#10872,#4611,.T.);
#13195=EDGE_CURVE('',#10871,#10873,#4612,.T.);
#13196=EDGE_CURVE('',#10872,#10875,#4613,.T.);
#13197=EDGE_CURVE('',#10876,#10875,#263,.T.);
#13198=EDGE_CURVE('',#10789,#10876,#264,.T.);
#13199=EDGE_CURVE('',#10877,#10874,#4614,.T.);
#13200=EDGE_CURVE('',#10875,#10877,#4615,.T.);
#13201=EDGE_CURVE('',#10878,#10876,#265,.T.);
#13202=EDGE_CURVE('',#10878,#10790,#266,.T.);
#13203=EDGE_CURVE('',#10875,#10879,#4616,.T.);
#13204=EDGE_CURVE('',#10879,#10878,#267,.T.);
#13205=EDGE_CURVE('',#10877,#10880,#4617,.F.);
#13206=EDGE_CURVE('',#10880,#10879,#4618,.T.);
#13207=EDGE_CURVE('',#10879,#10881,#4619,.T.);
#13208=EDGE_CURVE('',#10791,#10881,#268,.T.);
#13209=EDGE_CURVE('',#10882,#10880,#4620,.T.);
#13210=EDGE_CURVE('',#10881,#10882,#4621,.T.);
#13211=EDGE_CURVE('',#10808,#10868,#4622,.T.);
#13212=EDGE_CURVE('',#10770,#10866,#4623,.T.);
#13213=EDGE_CURVE('',#10883,#10884,#4624,.F.);
#13214=EDGE_CURVE('',#10884,#10885,#4625,.T.);
#13215=EDGE_CURVE('',#10885,#10886,#4626,.T.);
#13216=EDGE_CURVE('',#10886,#10883,#4627,.T.);
#13217=EDGE_CURVE('',#10887,#10775,#4628,.T.);
#13218=EDGE_CURVE('',#10775,#10886,#10344,.T.);
#13219=EDGE_CURVE('',#10885,#10887,#10345,.T.);
#13220=EDGE_CURVE('',#10888,#10776,#4629,.T.);
#13221=EDGE_CURVE('',#10887,#10888,#4630,.T.);
#13222=EDGE_CURVE('',#10889,#10890,#4631,.T.);
#13223=EDGE_CURVE('',#10890,#10776,#10346,.T.);
#13224=EDGE_CURVE('',#10888,#10889,#10347,.T.);
#13225=EDGE_CURVE('',#10891,#10892,#4632,.F.);
#13226=EDGE_CURVE('',#10892,#10890,#4633,.T.);
#13227=EDGE_CURVE('',#10889,#10891,#4634,.T.);
#13228=EDGE_CURVE('',#10891,#10884,#4635,.T.);
#13229=EDGE_CURVE('',#10893,#10894,#269,.F.);
#13230=EDGE_CURVE('',#10894,#10895,#10348,.T.);
#13231=EDGE_CURVE('',#10895,#10896,#270,.F.);
#13232=EDGE_CURVE('',#10896,#10893,#10349,.T.);
#13233=EDGE_CURVE('',#10897,#10894,#4636,.T.);
#13234=EDGE_CURVE('',#10898,#10897,#10350,.T.);
#13235=EDGE_CURVE('',#10895,#10898,#4637,.T.);
#13236=EDGE_CURVE('',#10806,#10899,#271,.T.);
#13237=EDGE_CURVE('',#10899,#10900,#10351,.T.);
#13238=EDGE_CURVE('',#10807,#10900,#272,.T.);
#13239=EDGE_CURVE('',#10805,#10901,#273,.T.);
#13240=EDGE_CURVE('',#10901,#10899,#10352,.T.);
#13241=EDGE_CURVE('',#10804,#10902,#10353,.T.);
#13242=EDGE_CURVE('',#10902,#10903,#10354,.T.);
#13243=EDGE_CURVE('',#10903,#10803,#10355,.T.);
#13244=EDGE_CURVE('',#10903,#10901,#4638,.T.);
#13245=EDGE_CURVE('',#10900,#10902,#4639,.T.);
#13246=EDGE_CURVE('',#10904,#10901,#4640,.T.);
#13247=EDGE_CURVE('',#10905,#10904,#10356,.T.);
#13248=EDGE_CURVE('',#10905,#10899,#4641,.T.);
#13249=EDGE_CURVE('',#10903,#10906,#4642,.T.);
#13250=EDGE_CURVE('',#10906,#10904,#4643,.T.);
#13251=EDGE_CURVE('',#10902,#10907,#4644,.T.);
#13252=EDGE_CURVE('',#10907,#10906,#10357,.T.);
#13253=EDGE_CURVE('',#10796,#10908,#274,.T.);
#13254=EDGE_CURVE('',#10908,#10909,#10358,.T.);
#13255=EDGE_CURVE('',#10797,#10909,#275,.T.);
#13256=EDGE_CURVE('',#10795,#10910,#276,.T.);
#13257=EDGE_CURVE('',#10910,#10908,#10359,.T.);
#13258=EDGE_CURVE('',#10794,#10911,#10360,.T.);
#13259=EDGE_CURVE('',#10911,#10912,#10361,.T.);
#13260=EDGE_CURVE('',#10912,#10793,#10362,.T.);
#13261=EDGE_CURVE('',#10912,#10910,#4645,.T.);
#13262=EDGE_CURVE('',#10909,#10911,#4646,.T.);
#13263=EDGE_CURVE('',#10913,#10910,#4647,.T.);
#13264=EDGE_CURVE('',#10914,#10913,#10363,.T.);
#13265=EDGE_CURVE('',#10914,#10908,#4648,.T.);
#13266=EDGE_CURVE('',#10912,#10915,#4649,.T.);
#13267=EDGE_CURVE('',#10915,#10913,#4650,.T.);
#13268=EDGE_CURVE('',#10911,#10916,#4651,.T.);
#13269=EDGE_CURVE('',#10916,#10915,#10364,.T.);
#13270=EDGE_CURVE('',#10769,#10898,#277,.F.);
#13271=EDGE_CURVE('',#10897,#10761,#278,.F.);
#13272=EDGE_CURVE('',#10815,#10917,#10365,.T.);
#13273=EDGE_CURVE('',#10917,#10774,#279,.F.);
#13274=EDGE_CURVE('',#10918,#10816,#10366,.T.);
#13275=EDGE_CURVE('',#10918,#10917,#4652,.T.);
#13276=EDGE_CURVE('',#10784,#10919,#280,.F.);
#13277=EDGE_CURVE('',#10919,#10920,#10367,.T.);
#13278=EDGE_CURVE('',#10920,#10785,#281,.F.);
#13279=EDGE_CURVE('',#10921,#10919,#4653,.T.);
#13280=EDGE_CURVE('',#10922,#10921,#10368,.T.);
#13281=EDGE_CURVE('',#10922,#10920,#4654,.T.);
#13282=EDGE_CURVE('',#10923,#10924,#4655,.T.);
#13283=EDGE_CURVE('',#10924,#10780,#10369,.T.);
#13284=EDGE_CURVE('',#10779,#10923,#282,.T.);
#13285=EDGE_CURVE('',#10778,#10925,#283,.T.);
#13286=EDGE_CURVE('',#10925,#10923,#10370,.T.);
#13287=EDGE_CURVE('',#10777,#10926,#284,.F.);
#13288=EDGE_CURVE('',#10926,#10925,#10371,.T.);
#13289=EDGE_CURVE('',#10927,#10781,#10372,.T.);
#13290=EDGE_CURVE('',#10924,#10927,#10373,.T.);
#13291=EDGE_CURVE('',#10928,#10782,#10374,.T.);
#13292=EDGE_CURVE('',#10927,#10928,#4656,.T.);
#13293=EDGE_CURVE('',#10929,#10783,#10375,.T.);
#13294=EDGE_CURVE('',#10928,#10929,#10376,.T.);
#13295=EDGE_CURVE('',#10929,#10919,#4657,.T.);
#13296=EDGE_CURVE('',#10929,#10930,#4658,.T.);
#13297=EDGE_CURVE('',#10930,#10921,#4659,.T.);
#13298=EDGE_CURVE('',#10928,#10931,#4660,.T.);
#13299=EDGE_CURVE('',#10931,#10930,#10377,.T.);
#13300=EDGE_CURVE('',#10927,#10932,#4661,.T.);
#13301=EDGE_CURVE('',#10932,#10931,#4662,.T.);
#13302=EDGE_CURVE('',#10924,#10933,#4663,.T.);
#13303=EDGE_CURVE('',#10933,#10932,#10378,.T.);
#13304=EDGE_CURVE('',#10923,#10934,#4664,.T.);
#13305=EDGE_CURVE('',#10934,#10933,#4665,.T.);
#13306=EDGE_CURVE('',#10935,#10925,#4666,.T.);
#13307=EDGE_CURVE('',#10934,#10935,#10379,.T.);
#13308=EDGE_CURVE('',#10926,#10936,#4667,.T.);
#13309=EDGE_CURVE('',#10935,#10936,#10380,.T.);
#13310=EDGE_CURVE('',#10762,#10937,#10381,.T.);
#13311=EDGE_CURVE('',#10937,#10938,#4668,.T.);
#13312=EDGE_CURVE('',#10938,#10763,#10382,.T.);
#13313=EDGE_CURVE('',#10939,#10764,#10383,.T.);
#13314=EDGE_CURVE('',#10938,#10939,#10384,.T.);
#13315=EDGE_CURVE('',#10940,#10765,#10385,.T.);
#13316=EDGE_CURVE('',#10939,#10940,#4669,.T.);
#13317=EDGE_CURVE('',#10941,#10766,#10386,.T.);
#13318=EDGE_CURVE('',#10940,#10941,#10387,.T.);
#13319=EDGE_CURVE('',#10942,#10767,#10388,.T.);
#13320=EDGE_CURVE('',#10941,#10942,#4670,.T.);
#13321=EDGE_CURVE('',#10943,#10768,#10389,.T.);
#13322=EDGE_CURVE('',#10942,#10943,#10390,.T.);
#13323=EDGE_CURVE('',#10943,#10898,#4671,.T.);
#13324=EDGE_CURVE('',#10760,#10944,#10391,.T.);
#13325=EDGE_CURVE('',#10944,#10937,#10392,.T.);
#13326=EDGE_CURVE('',#10897,#10944,#4672,.T.);
#13327=EDGE_CURVE('',#10940,#10945,#4673,.T.);
#13328=EDGE_CURVE('',#10946,#10945,#10393,.T.);
#13329=EDGE_CURVE('',#10941,#10946,#4674,.T.);
#13330=EDGE_CURVE('',#10939,#10947,#4675,.T.);
#13331=EDGE_CURVE('',#10945,#10947,#4676,.T.);
#13332=EDGE_CURVE('',#10938,#10948,#4677,.T.);
#13333=EDGE_CURVE('',#10947,#10948,#10394,.T.);
#13334=EDGE_CURVE('',#10937,#10949,#4678,.T.);
#13335=EDGE_CURVE('',#10948,#10949,#4679,.T.);
#13336=EDGE_CURVE('',#10944,#10950,#4680,.T.);
#13337=EDGE_CURVE('',#10949,#10950,#10395,.T.);
#13338=EDGE_CURVE('',#10890,#10926,#4681,.T.);
#13339=EDGE_CURVE('',#10936,#10892,#4682,.T.);
#13340=EDGE_CURVE('',#10917,#10886,#4683,.T.);
#13341=EDGE_CURVE('',#10883,#10918,#4684,.T.);
#13342=EDGE_CURVE('',#10881,#10951,#10396,.T.);
#13343=EDGE_CURVE('',#10951,#10792,#285,.F.);
#13344=EDGE_CURVE('',#10786,#10952,#286,.T.);
#13345=EDGE_CURVE('',#10952,#10871,#4685,.T.);
#13346=EDGE_CURVE('',#10920,#10952,#10397,.T.);
#13347=EDGE_CURVE('',#10953,#10882,#10398,.T.);
#13348=EDGE_CURVE('',#10953,#10951,#4686,.T.);
#13349=EDGE_CURVE('',#10954,#10952,#4687,.T.);
#13350=EDGE_CURVE('',#10873,#10954,#4688,.T.);
#13351=EDGE_CURVE('',#10954,#10922,#10399,.T.);
#13352=EDGE_CURVE('',#10847,#10946,#10400,.T.);
#13353=EDGE_CURVE('',#10945,#10846,#10401,.T.);
#13354=EDGE_CURVE('',#10947,#10848,#10402,.T.);
#13355=EDGE_CURVE('',#10948,#10849,#10403,.T.);
#13356=EDGE_CURVE('',#10949,#10850,#10404,.T.);
#13357=EDGE_CURVE('',#10950,#10851,#10405,.T.);
#13358=EDGE_CURVE('',#10955,#10852,#10406,.T.);
#13359=EDGE_CURVE('',#10950,#10955,#4689,.T.);
#13360=EDGE_CURVE('',#10956,#10853,#10407,.T.);
#13361=EDGE_CURVE('',#10955,#10956,#10408,.T.);
#13362=EDGE_CURVE('',#10956,#10946,#4690,.T.);
#13363=EDGE_CURVE('',#10957,#10957,#10409,.T.);
#13364=EDGE_CURVE('',#10957,#10958,#10410,.T.);
#13365=EDGE_CURVE('',#10958,#10958,#10411,.T.);
#13366=EDGE_CURVE('',#10843,#10824,#10412,.T.);
#13367=EDGE_CURVE('',#10799,#10844,#287,.F.);
#13368=EDGE_CURVE('',#10841,#10802,#288,.F.);
#13369=EDGE_CURVE('',#10831,#10842,#10413,.T.);
#13370=EDGE_CURVE('',#10801,#10834,#289,.F.);
#13371=EDGE_CURVE('',#10800,#10957,#4691,.T.);
#13372=EDGE_CURVE('',#10821,#10798,#290,.F.);
#13373=EDGE_CURVE('',#10959,#10959,#10414,.T.);
#13374=EDGE_CURVE('',#10951,#10756,#4692,.T.);
#13375=EDGE_CURVE('',#10758,#10953,#4693,.T.);
#13376=EDGE_CURVE('',#10827,#10830,#10415,.T.);
#13377=EDGE_CURVE('',#10838,#10837,#10416,.T.);
#13378=EDGE_CURVE('',#10858,#10960,#10417,.T.);
#13379=EDGE_CURVE('',#10960,#10961,#4694,.T.);
#13380=EDGE_CURVE('',#10961,#10857,#10418,.T.);
#13381=EDGE_CURVE('',#10962,#10859,#10419,.T.);
#13382=EDGE_CURVE('',#10961,#10962,#10420,.T.);
#13383=EDGE_CURVE('',#10963,#10860,#10421,.T.);
#13384=EDGE_CURVE('',#10962,#10963,#4695,.T.);
#13385=EDGE_CURVE('',#10963,#10960,#10422,.T.);
#13386=EDGE_CURVE('',#10961,#10964,#4696,.T.);
#13387=EDGE_CURVE('',#10964,#10965,#10423,.T.);
#13388=EDGE_CURVE('',#10962,#10965,#4697,.T.);
#13389=EDGE_CURVE('',#10960,#10966,#4698,.T.);
#13390=EDGE_CURVE('',#10966,#10964,#4699,.T.);
#13391=EDGE_CURVE('',#10749,#10967,#10424,.T.);
#13392=EDGE_CURVE('',#10967,#10968,#4700,.T.);
#13393=EDGE_CURVE('',#10968,#10748,#10425,.T.);
#13394=EDGE_CURVE('',#10969,#10750,#10426,.T.);
#13395=EDGE_CURVE('',#10968,#10969,#10427,.T.);
#13396=EDGE_CURVE('',#10970,#10751,#10428,.T.);
#13397=EDGE_CURVE('',#10969,#10970,#4701,.T.);
#13398=EDGE_CURVE('',#10970,#10967,#10429,.T.);
#13399=EDGE_CURVE('',#10968,#10971,#4702,.T.);
#13400=EDGE_CURVE('',#10971,#10972,#10430,.T.);
#13401=EDGE_CURVE('',#10969,#10972,#4703,.T.);
#13402=EDGE_CURVE('',#10967,#10973,#4704,.T.);
#13403=EDGE_CURVE('',#10973,#10971,#4705,.T.);
#13404=EDGE_CURVE('',#10970,#10974,#4706,.T.);
#13405=EDGE_CURVE('',#10974,#10973,#10431,.T.);
#13406=EDGE_CURVE('',#10972,#10974,#4707,.T.);
#13407=EDGE_CURVE('',#10963,#10975,#4708,.T.);
#13408=EDGE_CURVE('',#10975,#10966,#10432,.T.);
#13409=EDGE_CURVE('',#10965,#10975,#4709,.T.);
#13410=EDGE_CURVE('',#10861,#10976,#4710,.T.);
#13411=EDGE_CURVE('',#10976,#10976,#10433,.T.);
#13412=EDGE_CURVE('',#10862,#10977,#4711,.T.);
#13413=EDGE_CURVE('',#10977,#10977,#10434,.T.);
#13414=EDGE_CURVE('',#10978,#10978,#10435,.T.);
#13415=EDGE_CURVE('',#10979,#10979,#10436,.T.);
#13416=EDGE_CURVE('',#10978,#10980,#4712,.T.);
#13417=EDGE_CURVE('',#10980,#10980,#10437,.T.);
#13418=EDGE_CURVE('',#10981,#10981,#10438,.T.);
#13419=EDGE_CURVE('',#10981,#10746,#4713,.T.);
#13420=EDGE_CURVE('',#10959,#10979,#4714,.T.);
#13421=EDGE_CURVE('',#10982,#10914,#10439,.T.);
#13422=EDGE_CURVE('',#10909,#10982,#4715,.T.);
#13423=EDGE_CURVE('',#10983,#10905,#10440,.T.);
#13424=EDGE_CURVE('',#10900,#10983,#4716,.T.);
#13425=EDGE_CURVE('',#10893,#10896,#4717,.T.);
#13426=EDGE_CURVE('',#10943,#10955,#4718,.T.);
#13427=EDGE_CURVE('',#10983,#10907,#4719,.T.);
#13428=EDGE_CURVE('',#10982,#10916,#4720,.T.);
#13429=EDGE_CURVE('',#10942,#10956,#4721,.T.);
#13430=EDGE_CURVE('',#10984,#10984,#10441,.T.);
#13431=EDGE_CURVE('',#10984,#10985,#4722,.T.);
#13432=EDGE_CURVE('',#10985,#10985,#10442,.T.);
#13433=EDGE_CURVE('',#10985,#10986,#4723,.T.);
#13434=EDGE_CURVE('',#10986,#10986,#10443,.T.);
#13435=EDGE_CURVE('',#10987,#10987,#10444,.T.);
#13436=EDGE_CURVE('',#10988,#10988,#10445,.T.);
#13437=EDGE_CURVE('',#10988,#10989,#4724,.T.);
#13438=EDGE_CURVE('',#10989,#10989,#10446,.T.);
#13439=EDGE_CURVE('',#10989,#10990,#4725,.T.);
#13440=EDGE_CURVE('',#10990,#10990,#10447,.T.);
#13441=EDGE_CURVE('',#10991,#10991,#10448,.T.);
#13442=EDGE_CURVE('',#10992,#10993,#10449,.T.);
#13443=EDGE_CURVE('',#10993,#10994,#4726,.T.);
#13444=EDGE_CURVE('',#10994,#10995,#10450,.T.);
#13445=EDGE_CURVE('',#10995,#10992,#4727,.T.);
#13446=EDGE_CURVE('',#10996,#10997,#10451,.T.);
#13447=EDGE_CURVE('',#10997,#10995,#10452,.T.);
#13448=EDGE_CURVE('',#10994,#10996,#10453,.T.);
#13449=EDGE_CURVE('',#10998,#10999,#10454,.T.);
#13450=EDGE_CURVE('',#10999,#10997,#4728,.T.);
#13451=EDGE_CURVE('',#10996,#10998,#4729,.T.);
#13452=EDGE_CURVE('',#11000,#11001,#10455,.T.);
#13453=EDGE_CURVE('',#11001,#10999,#10456,.T.);
#13454=EDGE_CURVE('',#10998,#11000,#10457,.T.);
#13455=EDGE_CURVE('',#11002,#11003,#10458,.T.);
#13456=EDGE_CURVE('',#11003,#11001,#4730,.T.);
#13457=EDGE_CURVE('',#11000,#11002,#4731,.T.);
#13458=EDGE_CURVE('',#11004,#11005,#10459,.T.);
#13459=EDGE_CURVE('',#11005,#11003,#10460,.T.);
#13460=EDGE_CURVE('',#11002,#11004,#10461,.T.);
#13461=EDGE_CURVE('',#11006,#11007,#10462,.T.);
#13462=EDGE_CURVE('',#11007,#11005,#4732,.T.);
#13463=EDGE_CURVE('',#11004,#11006,#4733,.T.);
#13464=EDGE_CURVE('',#10992,#11007,#10463,.T.);
#13465=EDGE_CURVE('',#11006,#10993,#10464,.T.);
#13466=EDGE_CURVE('',#11008,#10998,#4734,.T.);
#13467=EDGE_CURVE('',#11009,#11008,#10465,.T.);
#13468=EDGE_CURVE('',#11009,#11000,#4735,.T.);
#13469=EDGE_CURVE('',#11010,#10996,#4736,.T.);
#13470=EDGE_CURVE('',#11008,#11010,#4737,.T.);
#13471=EDGE_CURVE('',#11011,#10994,#4738,.T.);
#13472=EDGE_CURVE('',#11010,#11011,#10466,.T.);
#13473=EDGE_CURVE('',#11012,#10993,#4739,.T.);
#13474=EDGE_CURVE('',#11011,#11012,#4740,.T.);
#13475=EDGE_CURVE('',#11013,#11013,#10467,.T.);
#13476=EDGE_CURVE('',#11014,#11014,#10468,.T.);
#13477=EDGE_CURVE('',#11015,#11015,#10469,.T.);
#13478=EDGE_CURVE('',#11016,#11017,#10470,.T.);
#13479=EDGE_CURVE('',#11017,#11016,#10471,.T.);
#13480=EDGE_CURVE('',#11018,#11018,#10472,.T.);
#13481=EDGE_CURVE('',#11019,#11019,#10473,.T.);
#13482=EDGE_CURVE('',#11020,#11020,#10474,.T.);
#13483=EDGE_CURVE('',#11021,#11021,#10475,.T.);
#13484=EDGE_CURVE('',#11022,#11011,#10476,.T.);
#13485=EDGE_CURVE('',#11012,#11023,#10477,.T.);
#13486=EDGE_CURVE('',#11023,#11022,#4741,.T.);
#13487=EDGE_CURVE('',#11024,#11025,#10478,.T.);
#13488=EDGE_CURVE('',#11025,#11023,#10479,.T.);
#13489=EDGE_CURVE('',#11012,#11024,#10480,.T.);
#13490=EDGE_CURVE('',#11026,#11027,#10481,.T.);
#13491=EDGE_CURVE('',#11027,#11025,#4742,.T.);
#13492=EDGE_CURVE('',#11024,#11026,#4743,.T.);
#13493=EDGE_CURVE('',#11028,#11029,#10482,.T.);
#13494=EDGE_CURVE('',#11029,#11027,#10483,.T.);
#13495=EDGE_CURVE('',#11026,#11028,#10484,.T.);
#13496=EDGE_CURVE('',#11009,#11030,#10485,.T.);
#13497=EDGE_CURVE('',#11030,#11029,#4744,.T.);
#13498=EDGE_CURVE('',#11028,#11009,#4745,.T.);
#13499=EDGE_CURVE('',#11008,#11031,#10486,.T.);
#13500=EDGE_CURVE('',#11031,#11030,#10487,.T.);
#13501=EDGE_CURVE('',#11010,#11032,#10488,.T.);
#13502=EDGE_CURVE('',#11032,#11031,#4746,.T.);
#13503=EDGE_CURVE('',#11022,#11032,#10489,.T.);
#13504=EDGE_CURVE('',#11028,#11002,#4747,.T.);
#13505=EDGE_CURVE('',#11026,#11004,#4748,.T.);
#13506=EDGE_CURVE('',#11024,#11006,#4749,.T.);
#13507=EDGE_CURVE('',#11033,#11033,#10490,.T.);
#13508=EDGE_CURVE('',#11034,#11034,#10491,.T.);
#13509=EDGE_CURVE('',#11035,#11036,#10492,.T.);
#13510=EDGE_CURVE('',#11036,#11035,#10493,.T.);
#13511=EDGE_CURVE('',#11037,#11037,#10494,.T.);
#13512=EDGE_CURVE('',#11038,#11038,#10495,.T.);
#13513=EDGE_CURVE('',#11039,#11039,#10496,.T.);
#13514=EDGE_CURVE('',#11040,#11040,#10497,.T.);
#13515=EDGE_CURVE('',#11014,#11041,#4750,.T.);
#13516=EDGE_CURVE('',#11041,#11041,#10498,.T.);
#13517=EDGE_CURVE('',#11015,#11042,#4751,.T.);
#13518=EDGE_CURVE('',#11042,#11042,#10499,.T.);
#13519=EDGE_CURVE('',#11033,#11043,#4752,.T.);
#13520=EDGE_CURVE('',#11043,#11043,#10500,.T.);
#13521=EDGE_CURVE('',#11034,#11044,#4753,.T.);
#13522=EDGE_CURVE('',#11044,#11044,#10501,.T.);
#13523=EDGE_CURVE('',#11040,#11021,#4754,.T.);
#13524=EDGE_CURVE('',#11039,#11020,#4755,.T.);
#13525=EDGE_CURVE('',#11038,#11019,#4756,.T.);
#13526=EDGE_CURVE('',#11037,#11018,#4757,.T.);
#13527=EDGE_CURVE('',#11045,#11045,#10502,.T.);
#13528=EDGE_CURVE('',#11045,#11046,#4758,.T.);
#13529=EDGE_CURVE('',#11047,#11046,#291,.T.);
#13530=EDGE_CURVE('',#11048,#11047,#292,.T.);
#13531=EDGE_CURVE('',#11046,#11048,#293,.T.);
#13532=EDGE_CURVE('',#11048,#11017,#4759,.T.);
#13533=EDGE_CURVE('',#11049,#11016,#4760,.T.);
#13534=EDGE_CURVE('',#11049,#11050,#294,.T.);
#13535=EDGE_CURVE('',#11050,#11051,#295,.T.);
#13536=EDGE_CURVE('',#11036,#11051,#4761,.T.);
#13537=EDGE_CURVE('',#11035,#11047,#4762,.T.);
#13538=EDGE_CURVE('',#11052,#11052,#10503,.T.);
#13539=EDGE_CURVE('',#11052,#10991,#4763,.T.);
#13540=EDGE_CURVE('',#11053,#11053,#10504,.T.);
#13541=EDGE_CURVE('',#11053,#11050,#4764,.T.);
#13542=EDGE_CURVE('',#11051,#11049,#296,.T.);
#13543=EDGE_CURVE('',#11013,#10987,#4765,.T.);
#13544=EDGE_CURVE('',#11054,#11054,#10505,.T.);
#13545=EDGE_CURVE('',#11054,#11055,#4766,.T.);
#13546=EDGE_CURVE('',#11055,#11055,#10506,.T.);
#13547=EDGE_CURVE('',#11056,#11056,#10507,.T.);
#13548=EDGE_CURVE('',#11054,#11057,#4767,.T.);
#13549=EDGE_CURVE('',#11057,#11057,#10508,.T.);
#13550=EDGE_CURVE('',#11058,#11059,#4768,.T.);
#13551=EDGE_CURVE('',#11059,#11060,#4769,.T.);
#13552=EDGE_CURVE('',#11060,#11061,#4770,.T.);
#13553=EDGE_CURVE('',#11061,#11058,#4771,.T.);
#13554=EDGE_CURVE('',#11062,#11063,#4772,.T.);
#13555=EDGE_CURVE('',#11063,#11059,#10509,.T.);
#13556=EDGE_CURVE('',#11058,#11062,#10510,.T.);
#13557=EDGE_CURVE('',#11064,#11065,#4773,.T.);
#13558=EDGE_CURVE('',#11065,#11063,#4774,.T.);
#13559=EDGE_CURVE('',#11062,#11064,#4775,.T.);
#13560=EDGE_CURVE('',#11060,#11065,#10511,.T.);
#13561=EDGE_CURVE('',#11064,#11061,#10512,.T.);
#13562=EDGE_CURVE('',#11058,#11066,#4776,.T.);
#13563=EDGE_CURVE('',#11066,#11067,#10513,.T.);
#13564=EDGE_CURVE('',#11062,#11067,#4777,.T.);
#13565=EDGE_CURVE('',#11061,#11068,#4778,.T.);
#13566=EDGE_CURVE('',#11068,#11066,#4779,.T.);
#13567=EDGE_CURVE('',#11069,#11070,#10514,.T.);
#13568=EDGE_CURVE('',#11071,#11069,#4780,.T.);
#13569=EDGE_CURVE('',#11072,#11071,#10515,.T.);
#13570=EDGE_CURVE('',#11073,#11072,#4781,.T.);
#13571=EDGE_CURVE('',#11074,#11073,#10516,.T.);
#13572=EDGE_CURVE('',#11075,#11074,#4782,.T.);
#13573=EDGE_CURVE('',#11076,#11075,#10517,.T.);
#13574=EDGE_CURVE('',#11070,#11076,#4783,.T.);
#13575=EDGE_CURVE('',#11077,#11077,#10518,.T.);
#13576=EDGE_CURVE('',#11078,#11078,#10519,.T.);
#13577=EDGE_CURVE('',#11079,#11079,#10520,.T.);
#13578=EDGE_CURVE('',#11080,#11080,#10521,.T.);
#13579=EDGE_CURVE('',#11081,#11081,#10522,.T.);
#13580=EDGE_CURVE('',#11082,#11082,#10523,.T.);
#13581=EDGE_CURVE('',#11083,#11084,#4784,.T.);
#13582=EDGE_CURVE('',#11084,#11085,#4785,.T.);
#13583=EDGE_CURVE('',#11085,#11086,#4786,.T.);
#13584=EDGE_CURVE('',#11086,#11083,#4787,.T.);
#13585=EDGE_CURVE('',#11087,#11088,#4788,.T.);
#13586=EDGE_CURVE('',#11088,#11084,#10524,.T.);
#13587=EDGE_CURVE('',#11083,#11087,#10525,.T.);
#13588=EDGE_CURVE('',#11089,#11090,#4789,.T.);
#13589=EDGE_CURVE('',#11090,#11088,#4790,.T.);
#13590=EDGE_CURVE('',#11087,#11089,#4791,.T.);
#13591=EDGE_CURVE('',#11085,#11090,#10526,.T.);
#13592=EDGE_CURVE('',#11089,#11086,#10527,.T.);
#13593=EDGE_CURVE('',#11083,#11091,#4792,.T.);
#13594=EDGE_CURVE('',#11091,#11092,#10528,.T.);
#13595=EDGE_CURVE('',#11087,#11092,#4793,.T.);
#13596=EDGE_CURVE('',#11086,#11093,#4794,.T.);
#13597=EDGE_CURVE('',#11093,#11091,#4795,.T.);
#13598=EDGE_CURVE('',#11094,#11095,#115,.T.);
#13599=EDGE_CURVE('',#11095,#11096,#4796,.T.);
#13600=EDGE_CURVE('',#11096,#11096,#10529,.T.);
#13601=EDGE_CURVE('',#11095,#11097,#116,.T.);
#13602=EDGE_CURVE('',#11097,#11094,#10530,.T.);
#13603=EDGE_CURVE('',#11094,#11098,#4797,.T.);
#13604=EDGE_CURVE('',#11099,#11098,#117,.T.);
#13605=EDGE_CURVE('',#11100,#11099,#118,.T.);
#13606=EDGE_CURVE('',#11100,#11101,#4798,.T.);
#13607=EDGE_CURVE('',#11102,#11101,#4799,.T.);
#13608=EDGE_CURVE('',#11103,#11102,#4800,.T.);
#13609=EDGE_CURVE('',#11103,#11104,#4801,.T.);
#13610=EDGE_CURVE('',#11104,#11097,#4802,.T.);
#13611=EDGE_CURVE('',#11096,#11105,#4803,.T.);
#13612=EDGE_CURVE('',#11105,#11105,#10531,.T.);
#13613=EDGE_CURVE('',#11099,#11106,#4804,.T.);
#13614=EDGE_CURVE('',#11106,#11106,#10532,.T.);
#13615=EDGE_CURVE('',#11098,#11100,#10533,.T.);
#13616=EDGE_CURVE('',#11106,#11107,#4805,.T.);
#13617=EDGE_CURVE('',#11107,#11107,#10534,.T.);
#13618=EDGE_CURVE('',#11108,#11109,#119,.T.);
#13619=EDGE_CURVE('',#11109,#11110,#4806,.T.);
#13620=EDGE_CURVE('',#11110,#11111,#10535,.T.);
#13621=EDGE_CURVE('',#11111,#11110,#10536,.T.);
#13622=EDGE_CURVE('',#11109,#11112,#120,.T.);
#13623=EDGE_CURVE('',#11112,#11108,#10537,.T.);
#13624=EDGE_CURVE('',#11108,#11113,#4807,.T.);
#13625=EDGE_CURVE('',#11114,#11113,#121,.T.);
#13626=EDGE_CURVE('',#11115,#11114,#122,.T.);
#13627=EDGE_CURVE('',#11115,#11116,#4808,.T.);
#13628=EDGE_CURVE('',#11116,#11117,#4809,.T.);
#13629=EDGE_CURVE('',#11118,#11117,#4810,.T.);
#13630=EDGE_CURVE('',#11118,#11119,#4811,.T.);
#13631=EDGE_CURVE('',#11119,#11112,#4812,.T.);
#13632=EDGE_CURVE('',#11111,#11120,#4813,.T.);
#13633=EDGE_CURVE('',#11120,#11120,#10538,.T.);
#13634=EDGE_CURVE('',#11114,#11121,#4814,.T.);
#13635=EDGE_CURVE('',#11121,#11122,#10539,.T.);
#13636=EDGE_CURVE('',#11122,#11121,#10540,.T.);
#13637=EDGE_CURVE('',#11113,#11115,#10541,.T.);
#13638=EDGE_CURVE('',#11122,#11123,#4815,.T.);
#13639=EDGE_CURVE('',#11123,#11123,#10542,.T.);
#13640=EDGE_CURVE('',#11070,#11124,#4816,.T.);
#13641=EDGE_CURVE('',#11124,#11125,#10543,.T.);
#13642=EDGE_CURVE('',#11125,#11069,#4817,.T.);
#13643=EDGE_CURVE('',#11076,#11126,#4818,.T.);
#13644=EDGE_CURVE('',#11126,#11124,#4819,.T.);
#13645=EDGE_CURVE('',#11075,#11127,#4820,.T.);
#13646=EDGE_CURVE('',#11127,#11126,#10544,.T.);
#13647=EDGE_CURVE('',#11074,#11128,#4821,.T.);
#13648=EDGE_CURVE('',#11128,#11127,#4822,.T.);
#13649=EDGE_CURVE('',#11073,#11129,#4823,.T.);
#13650=EDGE_CURVE('',#11129,#11128,#10545,.T.);
#13651=EDGE_CURVE('',#11072,#11130,#4824,.T.);
#13652=EDGE_CURVE('',#11130,#11129,#4825,.T.);
#13653=EDGE_CURVE('',#11071,#11131,#4826,.T.);
#13654=EDGE_CURVE('',#11131,#11130,#10546,.T.);
#13655=EDGE_CURVE('',#11125,#11131,#4827,.T.);
#13656=EDGE_CURVE('',#11130,#11132,#4828,.T.);
#13657=EDGE_CURVE('',#11133,#11132,#4829,.T.);
#13658=EDGE_CURVE('',#11129,#11133,#4830,.T.);
#13659=EDGE_CURVE('',#11131,#11134,#4831,.T.);
#13660=EDGE_CURVE('',#11132,#11134,#10547,.T.);
#13661=EDGE_CURVE('',#11125,#11135,#4832,.T.);
#13662=EDGE_CURVE('',#11134,#11135,#4833,.T.);
#13663=EDGE_CURVE('',#11124,#11136,#4834,.T.);
#13664=EDGE_CURVE('',#11135,#11136,#10548,.T.);
#13665=EDGE_CURVE('',#11132,#11118,#4835,.T.);
#13666=EDGE_CURVE('',#11117,#11133,#4836,.T.);
#13667=EDGE_CURVE('',#11134,#11137,#4837,.T.);
#13668=EDGE_CURVE('',#11137,#11118,#10549,.T.);
#13669=EDGE_CURVE('',#11135,#11138,#4838,.T.);
#13670=EDGE_CURVE('',#11138,#11137,#4839,.T.);
#13671=EDGE_CURVE('',#11136,#11102,#4840,.T.);
#13672=EDGE_CURVE('',#11102,#11138,#10550,.T.);
#13673=EDGE_CURVE('',#11139,#11103,#4841,.T.);
#13674=EDGE_CURVE('',#11136,#11139,#4842,.T.);
#13675=EDGE_CURVE('',#11140,#11141,#4843,.T.);
#13676=EDGE_CURVE('',#11141,#11103,#10551,.T.);
#13677=EDGE_CURVE('',#11139,#11140,#10552,.T.);
#13678=EDGE_CURVE('',#11142,#11143,#4844,.T.);
#13679=EDGE_CURVE('',#11143,#11141,#4845,.T.);
#13680=EDGE_CURVE('',#11140,#11142,#4846,.T.);
#13681=EDGE_CURVE('',#11117,#11143,#10553,.T.);
#13682=EDGE_CURVE('',#11142,#11133,#10554,.T.);
#13683=EDGE_CURVE('',#11141,#11144,#4847,.T.);
#13684=EDGE_CURVE('',#11144,#11104,#10555,.T.);
#13685=EDGE_CURVE('',#11143,#11145,#4848,.T.);
#13686=EDGE_CURVE('',#11145,#11144,#4849,.T.);
#13687=EDGE_CURVE('',#11116,#11145,#10556,.T.);
#13688=EDGE_CURVE('',#11137,#11146,#4850,.T.);
#13689=EDGE_CURVE('',#11146,#11119,#10557,.T.);
#13690=EDGE_CURVE('',#11138,#11147,#4851,.T.);
#13691=EDGE_CURVE('',#11147,#11146,#4852,.T.);
#13692=EDGE_CURVE('',#11101,#11147,#10558,.T.);
#13693=EDGE_CURVE('',#11148,#11148,#10559,.T.);
#13694=EDGE_CURVE('',#11089,#11149,#4853,.T.);
#13695=EDGE_CURVE('',#11149,#11093,#10560,.T.);
#13696=EDGE_CURVE('',#11092,#11149,#4854,.T.);
#13697=EDGE_CURVE('',#11064,#11150,#4855,.T.);
#13698=EDGE_CURVE('',#11150,#11068,#10561,.T.);
#13699=EDGE_CURVE('',#11067,#11150,#4856,.T.);
#13700=EDGE_CURVE('',#11148,#11056,#4857,.T.);
#13701=EDGE_CURVE('',#11082,#11151,#4858,.T.);
#13702=EDGE_CURVE('',#11151,#11151,#10562,.T.);
#13703=EDGE_CURVE('',#11081,#11152,#4859,.T.);
#13704=EDGE_CURVE('',#11152,#11152,#10563,.T.);
#13705=EDGE_CURVE('',#11153,#11153,#10564,.T.);
#13706=EDGE_CURVE('',#11153,#11080,#4860,.T.);
#13707=EDGE_CURVE('',#11154,#11154,#10565,.T.);
#13708=EDGE_CURVE('',#11154,#11079,#4861,.T.);
#13709=EDGE_CURVE('',#11155,#11155,#10566,.T.);
#13710=EDGE_CURVE('',#11155,#11078,#4862,.T.);
#13711=EDGE_CURVE('',#11156,#11156,#10567,.T.);
#13712=EDGE_CURVE('',#11156,#11077,#4863,.T.);
#13713=EDGE_CURVE('',#11128,#11142,#4864,.T.);
#13714=EDGE_CURVE('',#11127,#11140,#4865,.T.);
#13715=EDGE_CURVE('',#11126,#11139,#4866,.T.);
#13716=EDGE_CURVE('',#11157,#11158,#4867,.T.);
#13717=EDGE_CURVE('',#11158,#11159,#4868,.T.);
#13718=EDGE_CURVE('',#11159,#11160,#4869,.F.);
#13719=EDGE_CURVE('',#11160,#11161,#4870,.T.);
#13720=EDGE_CURVE('',#11161,#11162,#4871,.T.);
#13721=EDGE_CURVE('',#11162,#11157,#4872,.T.);
#13722=EDGE_CURVE('',#11163,#11159,#4873,.T.);
#13723=EDGE_CURVE('',#11158,#11164,#4874,.T.);
#13724=EDGE_CURVE('',#11164,#11165,#4875,.T.);
#13725=EDGE_CURVE('',#11165,#11166,#4876,.T.);
#13726=EDGE_CURVE('',#11166,#11167,#4877,.T.);
#13727=EDGE_CURVE('',#11167,#11168,#4878,.T.);
#13728=EDGE_CURVE('',#11168,#11169,#4879,.T.);
#13729=EDGE_CURVE('',#11169,#11170,#4880,.T.);
#13730=EDGE_CURVE('',#11170,#11171,#4881,.T.);
#13731=EDGE_CURVE('',#11171,#11172,#4882,.T.);
#13732=EDGE_CURVE('',#11172,#11173,#4883,.T.);
#13733=EDGE_CURVE('',#11173,#11174,#4884,.T.);
#13734=EDGE_CURVE('',#11174,#11175,#4885,.T.);
#13735=EDGE_CURVE('',#11175,#11176,#4886,.T.);
#13736=EDGE_CURVE('',#11176,#11177,#4887,.T.);
#13737=EDGE_CURVE('',#11177,#11178,#4888,.T.);
#13738=EDGE_CURVE('',#11178,#11179,#4889,.T.);
#13739=EDGE_CURVE('',#11180,#11179,#4890,.T.);
#13740=EDGE_CURVE('',#11180,#11181,#4891,.T.);
#13741=EDGE_CURVE('',#11181,#11182,#4892,.T.);
#13742=EDGE_CURVE('',#11183,#11182,#4893,.T.);
#13743=EDGE_CURVE('',#11183,#11184,#4894,.T.);
#13744=EDGE_CURVE('',#11184,#11185,#4895,.T.);
#13745=EDGE_CURVE('',#11185,#11186,#4896,.T.);
#13746=EDGE_CURVE('',#11186,#11187,#4897,.T.);
#13747=EDGE_CURVE('',#11187,#11188,#4898,.T.);
#13748=EDGE_CURVE('',#11188,#11189,#4899,.T.);
#13749=EDGE_CURVE('',#11189,#11190,#4900,.T.);
#13750=EDGE_CURVE('',#11190,#11191,#4901,.T.);
#13751=EDGE_CURVE('',#11191,#11192,#4902,.T.);
#13752=EDGE_CURVE('',#11192,#11193,#4903,.T.);
#13753=EDGE_CURVE('',#11193,#11194,#4904,.T.);
#13754=EDGE_CURVE('',#11194,#11195,#4905,.T.);
#13755=EDGE_CURVE('',#11195,#11196,#4906,.T.);
#13756=EDGE_CURVE('',#11196,#11197,#4907,.T.);
#13757=EDGE_CURVE('',#11197,#11198,#4908,.T.);
#13758=EDGE_CURVE('',#11198,#11199,#4909,.T.);
#13759=EDGE_CURVE('',#11200,#11199,#4910,.T.);
#13760=EDGE_CURVE('',#11200,#11201,#4911,.T.);
#13761=EDGE_CURVE('',#11201,#11202,#4912,.T.);
#13762=EDGE_CURVE('',#11203,#11202,#4913,.T.);
#13763=EDGE_CURVE('',#11203,#11204,#4914,.T.);
#13764=EDGE_CURVE('',#11204,#11205,#4915,.T.);
#13765=EDGE_CURVE('',#11205,#11206,#4916,.T.);
#13766=EDGE_CURVE('',#11206,#11207,#4917,.T.);
#13767=EDGE_CURVE('',#11207,#11208,#4918,.T.);
#13768=EDGE_CURVE('',#11208,#11209,#4919,.T.);
#13769=EDGE_CURVE('',#11209,#11210,#4920,.T.);
#13770=EDGE_CURVE('',#11210,#11211,#4921,.T.);
#13771=EDGE_CURVE('',#11211,#11212,#4922,.T.);
#13772=EDGE_CURVE('',#11212,#11213,#4923,.T.);
#13773=EDGE_CURVE('',#11213,#11214,#4924,.T.);
#13774=EDGE_CURVE('',#11214,#11215,#4925,.T.);
#13775=EDGE_CURVE('',#11215,#11216,#4926,.T.);
#13776=EDGE_CURVE('',#11216,#11217,#4927,.T.);
#13777=EDGE_CURVE('',#11217,#11218,#4928,.T.);
#13778=EDGE_CURVE('',#11218,#11219,#4929,.T.);
#13779=EDGE_CURVE('',#11220,#11219,#4930,.T.);
#13780=EDGE_CURVE('',#11220,#11221,#4931,.T.);
#13781=EDGE_CURVE('',#11221,#11222,#4932,.T.);
#13782=EDGE_CURVE('',#11223,#11222,#4933,.T.);
#13783=EDGE_CURVE('',#11223,#11224,#4934,.T.);
#13784=EDGE_CURVE('',#11224,#11225,#4935,.T.);
#13785=EDGE_CURVE('',#11225,#11226,#4936,.T.);
#13786=EDGE_CURVE('',#11226,#11227,#4937,.T.);
#13787=EDGE_CURVE('',#11227,#11228,#4938,.T.);
#13788=EDGE_CURVE('',#11228,#11229,#4939,.T.);
#13789=EDGE_CURVE('',#11229,#11230,#4940,.T.);
#13790=EDGE_CURVE('',#11230,#11231,#4941,.T.);
#13791=EDGE_CURVE('',#11231,#11232,#4942,.T.);
#13792=EDGE_CURVE('',#11232,#11233,#4943,.T.);
#13793=EDGE_CURVE('',#11233,#11234,#4944,.T.);
#13794=EDGE_CURVE('',#11234,#11235,#4945,.T.);
#13795=EDGE_CURVE('',#11235,#11236,#4946,.T.);
#13796=EDGE_CURVE('',#11236,#11237,#4947,.T.);
#13797=EDGE_CURVE('',#11237,#11238,#4948,.T.);
#13798=EDGE_CURVE('',#11238,#11239,#4949,.T.);
#13799=EDGE_CURVE('',#11240,#11239,#4950,.T.);
#13800=EDGE_CURVE('',#11240,#11241,#4951,.T.);
#13801=EDGE_CURVE('',#11241,#11242,#4952,.T.);
#13802=EDGE_CURVE('',#11243,#11242,#4953,.T.);
#13803=EDGE_CURVE('',#11243,#11244,#4954,.T.);
#13804=EDGE_CURVE('',#11244,#11245,#4955,.T.);
#13805=EDGE_CURVE('',#11245,#11246,#4956,.T.);
#13806=EDGE_CURVE('',#11246,#11247,#4957,.T.);
#13807=EDGE_CURVE('',#11247,#11248,#4958,.T.);
#13808=EDGE_CURVE('',#11248,#11249,#4959,.T.);
#13809=EDGE_CURVE('',#11249,#11250,#4960,.T.);
#13810=EDGE_CURVE('',#11250,#11251,#4961,.T.);
#13811=EDGE_CURVE('',#11251,#11252,#4962,.T.);
#13812=EDGE_CURVE('',#11252,#11253,#4963,.T.);
#13813=EDGE_CURVE('',#11253,#11254,#4964,.T.);
#13814=EDGE_CURVE('',#11254,#11255,#4965,.T.);
#13815=EDGE_CURVE('',#11255,#11256,#4966,.T.);
#13816=EDGE_CURVE('',#11256,#11257,#4967,.T.);
#13817=EDGE_CURVE('',#11257,#11258,#4968,.T.);
#13818=EDGE_CURVE('',#11258,#11259,#4969,.T.);
#13819=EDGE_CURVE('',#11260,#11259,#4970,.T.);
#13820=EDGE_CURVE('',#11260,#11261,#4971,.T.);
#13821=EDGE_CURVE('',#11261,#11262,#4972,.T.);
#13822=EDGE_CURVE('',#11263,#11262,#4973,.T.);
#13823=EDGE_CURVE('',#11263,#11264,#4974,.T.);
#13824=EDGE_CURVE('',#11264,#11265,#4975,.T.);
#13825=EDGE_CURVE('',#11265,#11266,#4976,.T.);
#13826=EDGE_CURVE('',#11266,#11267,#4977,.T.);
#13827=EDGE_CURVE('',#11267,#11268,#4978,.T.);
#13828=EDGE_CURVE('',#11268,#11269,#4979,.T.);
#13829=EDGE_CURVE('',#11269,#11270,#4980,.T.);
#13830=EDGE_CURVE('',#11270,#11271,#4981,.T.);
#13831=EDGE_CURVE('',#11271,#11272,#4982,.T.);
#13832=EDGE_CURVE('',#11272,#11273,#4983,.T.);
#13833=EDGE_CURVE('',#11273,#11274,#4984,.T.);
#13834=EDGE_CURVE('',#11274,#11275,#4985,.T.);
#13835=EDGE_CURVE('',#11275,#11276,#4986,.T.);
#13836=EDGE_CURVE('',#11276,#11277,#4987,.T.);
#13837=EDGE_CURVE('',#11277,#11278,#4988,.T.);
#13838=EDGE_CURVE('',#11278,#11279,#4989,.T.);
#13839=EDGE_CURVE('',#11280,#11279,#4990,.T.);
#13840=EDGE_CURVE('',#11280,#11281,#4991,.T.);
#13841=EDGE_CURVE('',#11281,#11282,#4992,.T.);
#13842=EDGE_CURVE('',#11283,#11282,#4993,.T.);
#13843=EDGE_CURVE('',#11283,#11284,#4994,.T.);
#13844=EDGE_CURVE('',#11284,#11285,#4995,.T.);
#13845=EDGE_CURVE('',#11285,#11286,#4996,.T.);
#13846=EDGE_CURVE('',#11286,#11287,#4997,.T.);
#13847=EDGE_CURVE('',#11287,#11288,#4998,.T.);
#13848=EDGE_CURVE('',#11288,#11289,#4999,.T.);
#13849=EDGE_CURVE('',#11289,#11290,#5000,.T.);
#13850=EDGE_CURVE('',#11290,#11291,#5001,.T.);
#13851=EDGE_CURVE('',#11291,#11292,#5002,.T.);
#13852=EDGE_CURVE('',#11292,#11293,#5003,.T.);
#13853=EDGE_CURVE('',#11293,#11294,#5004,.T.);
#13854=EDGE_CURVE('',#11294,#11295,#5005,.T.);
#13855=EDGE_CURVE('',#11295,#11296,#5006,.T.);
#13856=EDGE_CURVE('',#11296,#11297,#5007,.T.);
#13857=EDGE_CURVE('',#11297,#11298,#5008,.T.);
#13858=EDGE_CURVE('',#11298,#11299,#5009,.T.);
#13859=EDGE_CURVE('',#11300,#11299,#5010,.T.);
#13860=EDGE_CURVE('',#11300,#11301,#5011,.T.);
#13861=EDGE_CURVE('',#11301,#11302,#5012,.T.);
#13862=EDGE_CURVE('',#11303,#11302,#5013,.T.);
#13863=EDGE_CURVE('',#11303,#11304,#5014,.T.);
#13864=EDGE_CURVE('',#11304,#11305,#5015,.T.);
#13865=EDGE_CURVE('',#11305,#11306,#5016,.T.);
#13866=EDGE_CURVE('',#11306,#11307,#5017,.T.);
#13867=EDGE_CURVE('',#11307,#11308,#5018,.T.);
#13868=EDGE_CURVE('',#11308,#11309,#5019,.T.);
#13869=EDGE_CURVE('',#11309,#11310,#5020,.T.);
#13870=EDGE_CURVE('',#11310,#11311,#5021,.T.);
#13871=EDGE_CURVE('',#11311,#11312,#5022,.T.);
#13872=EDGE_CURVE('',#11312,#11313,#5023,.T.);
#13873=EDGE_CURVE('',#11313,#11314,#5024,.T.);
#13874=EDGE_CURVE('',#11314,#11315,#5025,.T.);
#13875=EDGE_CURVE('',#11315,#11316,#5026,.T.);
#13876=EDGE_CURVE('',#11316,#11317,#5027,.T.);
#13877=EDGE_CURVE('',#11317,#11318,#5028,.T.);
#13878=EDGE_CURVE('',#11318,#11319,#5029,.T.);
#13879=EDGE_CURVE('',#11320,#11319,#5030,.T.);
#13880=EDGE_CURVE('',#11320,#11321,#5031,.T.);
#13881=EDGE_CURVE('',#11321,#11322,#5032,.T.);
#13882=EDGE_CURVE('',#11323,#11322,#5033,.T.);
#13883=EDGE_CURVE('',#11323,#11324,#5034,.T.);
#13884=EDGE_CURVE('',#11324,#11325,#5035,.T.);
#13885=EDGE_CURVE('',#11325,#11326,#5036,.T.);
#13886=EDGE_CURVE('',#11326,#11327,#5037,.T.);
#13887=EDGE_CURVE('',#11327,#11328,#5038,.T.);
#13888=EDGE_CURVE('',#11328,#11329,#5039,.T.);
#13889=EDGE_CURVE('',#11329,#11330,#5040,.T.);
#13890=EDGE_CURVE('',#11330,#11331,#5041,.T.);
#13891=EDGE_CURVE('',#11331,#11332,#5042,.T.);
#13892=EDGE_CURVE('',#11332,#11333,#5043,.T.);
#13893=EDGE_CURVE('',#11333,#11334,#5044,.T.);
#13894=EDGE_CURVE('',#11334,#11335,#5045,.T.);
#13895=EDGE_CURVE('',#11335,#11336,#5046,.T.);
#13896=EDGE_CURVE('',#11336,#11337,#5047,.T.);
#13897=EDGE_CURVE('',#11337,#11338,#5048,.T.);
#13898=EDGE_CURVE('',#11338,#11339,#5049,.T.);
#13899=EDGE_CURVE('',#11340,#11339,#5050,.T.);
#13900=EDGE_CURVE('',#11340,#11341,#5051,.T.);
#13901=EDGE_CURVE('',#11341,#11342,#5052,.T.);
#13902=EDGE_CURVE('',#11343,#11342,#5053,.T.);
#13903=EDGE_CURVE('',#11343,#11344,#5054,.T.);
#13904=EDGE_CURVE('',#11344,#11345,#5055,.T.);
#13905=EDGE_CURVE('',#11345,#11346,#5056,.T.);
#13906=EDGE_CURVE('',#11346,#11347,#5057,.T.);
#13907=EDGE_CURVE('',#11347,#11348,#5058,.T.);
#13908=EDGE_CURVE('',#11348,#11349,#5059,.T.);
#13909=EDGE_CURVE('',#11349,#11350,#5060,.T.);
#13910=EDGE_CURVE('',#11350,#11351,#5061,.T.);
#13911=EDGE_CURVE('',#11351,#11352,#5062,.T.);
#13912=EDGE_CURVE('',#11352,#11353,#5063,.T.);
#13913=EDGE_CURVE('',#11353,#11354,#5064,.T.);
#13914=EDGE_CURVE('',#11354,#11355,#5065,.T.);
#13915=EDGE_CURVE('',#11355,#11356,#5066,.T.);
#13916=EDGE_CURVE('',#11356,#11357,#5067,.T.);
#13917=EDGE_CURVE('',#11357,#11358,#5068,.T.);
#13918=EDGE_CURVE('',#11358,#11359,#5069,.T.);
#13919=EDGE_CURVE('',#11360,#11359,#5070,.T.);
#13920=EDGE_CURVE('',#11360,#11361,#5071,.T.);
#13921=EDGE_CURVE('',#11361,#11362,#5072,.T.);
#13922=EDGE_CURVE('',#11363,#11362,#5073,.T.);
#13923=EDGE_CURVE('',#11363,#11364,#5074,.T.);
#13924=EDGE_CURVE('',#11364,#11365,#5075,.T.);
#13925=EDGE_CURVE('',#11365,#11366,#5076,.T.);
#13926=EDGE_CURVE('',#11366,#11367,#5077,.T.);
#13927=EDGE_CURVE('',#11367,#11368,#5078,.T.);
#13928=EDGE_CURVE('',#11368,#11369,#5079,.T.);
#13929=EDGE_CURVE('',#11369,#11370,#5080,.T.);
#13930=EDGE_CURVE('',#11370,#11371,#5081,.T.);
#13931=EDGE_CURVE('',#11371,#11372,#5082,.T.);
#13932=EDGE_CURVE('',#11372,#11373,#5083,.T.);
#13933=EDGE_CURVE('',#11373,#11374,#5084,.T.);
#13934=EDGE_CURVE('',#11374,#11375,#5085,.T.);
#13935=EDGE_CURVE('',#11375,#11376,#5086,.T.);
#13936=EDGE_CURVE('',#11376,#11377,#5087,.T.);
#13937=EDGE_CURVE('',#11377,#11378,#5088,.T.);
#13938=EDGE_CURVE('',#11378,#11379,#5089,.T.);
#13939=EDGE_CURVE('',#11380,#11379,#5090,.T.);
#13940=EDGE_CURVE('',#11380,#11381,#5091,.T.);
#13941=EDGE_CURVE('',#11381,#11382,#5092,.T.);
#13942=EDGE_CURVE('',#11383,#11382,#5093,.T.);
#13943=EDGE_CURVE('',#11383,#11384,#5094,.T.);
#13944=EDGE_CURVE('',#11384,#11385,#5095,.T.);
#13945=EDGE_CURVE('',#11385,#11386,#5096,.T.);
#13946=EDGE_CURVE('',#11386,#11387,#5097,.T.);
#13947=EDGE_CURVE('',#11387,#11388,#5098,.T.);
#13948=EDGE_CURVE('',#11388,#11389,#5099,.T.);
#13949=EDGE_CURVE('',#11389,#11390,#5100,.T.);
#13950=EDGE_CURVE('',#11390,#11391,#5101,.T.);
#13951=EDGE_CURVE('',#11391,#11392,#5102,.T.);
#13952=EDGE_CURVE('',#11392,#11393,#5103,.T.);
#13953=EDGE_CURVE('',#11393,#11394,#5104,.T.);
#13954=EDGE_CURVE('',#11394,#11395,#5105,.T.);
#13955=EDGE_CURVE('',#11395,#11396,#5106,.T.);
#13956=EDGE_CURVE('',#11396,#11397,#5107,.T.);
#13957=EDGE_CURVE('',#11397,#11398,#5108,.T.);
#13958=EDGE_CURVE('',#11398,#11399,#5109,.T.);
#13959=EDGE_CURVE('',#11400,#11399,#5110,.T.);
#13960=EDGE_CURVE('',#11400,#11163,#5111,.T.);
#13961=EDGE_CURVE('',#11401,#11401,#10568,.T.);
#13962=EDGE_CURVE('',#11157,#11402,#5112,.T.);
#13963=EDGE_CURVE('',#11403,#11402,#5113,.T.);
#13964=EDGE_CURVE('',#11404,#11403,#5114,.T.);
#13965=EDGE_CURVE('',#11164,#11404,#5115,.T.);
#13966=EDGE_CURVE('',#11162,#11405,#5116,.T.);
#13967=EDGE_CURVE('',#11402,#11405,#5117,.T.);
#13968=EDGE_CURVE('',#11406,#11383,#5118,.T.);
#13969=EDGE_CURVE('',#11382,#11407,#5119,.F.);
#13970=EDGE_CURVE('',#11407,#11408,#5120,.T.);
#13971=EDGE_CURVE('',#11408,#11409,#5121,.T.);
#13972=EDGE_CURVE('',#11409,#11406,#5122,.T.);
#13973=EDGE_CURVE('',#11406,#11410,#5123,.T.);
#13974=EDGE_CURVE('',#11411,#11410,#5124,.T.);
#13975=EDGE_CURVE('',#11412,#11411,#5125,.T.);
#13976=EDGE_CURVE('',#11384,#11412,#5126,.T.);
#13977=EDGE_CURVE('',#11409,#11413,#5127,.T.);
#13978=EDGE_CURVE('',#11410,#11413,#5128,.T.);
#13979=EDGE_CURVE('',#11414,#11363,#5129,.T.);
#13980=EDGE_CURVE('',#11362,#11415,#5130,.F.);
#13981=EDGE_CURVE('',#11415,#11416,#5131,.T.);
#13982=EDGE_CURVE('',#11416,#11417,#5132,.T.);
#13983=EDGE_CURVE('',#11417,#11414,#5133,.T.);
#13984=EDGE_CURVE('',#11414,#11418,#5134,.T.);
#13985=EDGE_CURVE('',#11419,#11418,#5135,.T.);
#13986=EDGE_CURVE('',#11420,#11419,#5136,.T.);
#13987=EDGE_CURVE('',#11364,#11420,#5137,.T.);
#13988=EDGE_CURVE('',#11417,#11421,#5138,.T.);
#13989=EDGE_CURVE('',#11418,#11421,#5139,.T.);
#13990=EDGE_CURVE('',#11422,#11343,#5140,.T.);
#13991=EDGE_CURVE('',#11342,#11423,#5141,.F.);
#13992=EDGE_CURVE('',#11423,#11424,#5142,.T.);
#13993=EDGE_CURVE('',#11424,#11425,#5143,.T.);
#13994=EDGE_CURVE('',#11425,#11422,#5144,.T.);
#13995=EDGE_CURVE('',#11422,#11426,#5145,.T.);
#13996=EDGE_CURVE('',#11427,#11426,#5146,.T.);
#13997=EDGE_CURVE('',#11428,#11427,#5147,.T.);
#13998=EDGE_CURVE('',#11344,#11428,#5148,.T.);
#13999=EDGE_CURVE('',#11425,#11429,#5149,.T.);
#14000=EDGE_CURVE('',#11426,#11429,#5150,.T.);
#14001=EDGE_CURVE('',#11430,#11323,#5151,.T.);
#14002=EDGE_CURVE('',#11322,#11431,#5152,.F.);
#14003=EDGE_CURVE('',#11431,#11432,#5153,.T.);
#14004=EDGE_CURVE('',#11432,#11433,#5154,.T.);
#14005=EDGE_CURVE('',#11433,#11430,#5155,.T.);
#14006=EDGE_CURVE('',#11430,#11434,#5156,.T.);
#14007=EDGE_CURVE('',#11435,#11434,#5157,.T.);
#14008=EDGE_CURVE('',#11436,#11435,#5158,.T.);
#14009=EDGE_CURVE('',#11324,#11436,#5159,.T.);
#14010=EDGE_CURVE('',#11433,#11437,#5160,.T.);
#14011=EDGE_CURVE('',#11434,#11437,#5161,.T.);
#14012=EDGE_CURVE('',#11438,#11303,#5162,.T.);
#14013=EDGE_CURVE('',#11302,#11439,#5163,.F.);
#14014=EDGE_CURVE('',#11439,#11440,#5164,.T.);
#14015=EDGE_CURVE('',#11440,#11441,#5165,.T.);
#14016=EDGE_CURVE('',#11441,#11438,#5166,.T.);
#14017=EDGE_CURVE('',#11438,#11442,#5167,.T.);
#14018=EDGE_CURVE('',#11443,#11442,#5168,.T.);
#14019=EDGE_CURVE('',#11444,#11443,#5169,.T.);
#14020=EDGE_CURVE('',#11304,#11444,#5170,.T.);
#14021=EDGE_CURVE('',#11441,#11445,#5171,.T.);
#14022=EDGE_CURVE('',#11442,#11445,#5172,.T.);
#14023=EDGE_CURVE('',#11446,#11283,#5173,.T.);
#14024=EDGE_CURVE('',#11282,#11447,#5174,.F.);
#14025=EDGE_CURVE('',#11447,#11448,#5175,.T.);
#14026=EDGE_CURVE('',#11448,#11449,#5176,.T.);
#14027=EDGE_CURVE('',#11449,#11446,#5177,.T.);
#14028=EDGE_CURVE('',#11446,#11450,#5178,.T.);
#14029=EDGE_CURVE('',#11451,#11450,#5179,.T.);
#14030=EDGE_CURVE('',#11452,#11451,#5180,.T.);
#14031=EDGE_CURVE('',#11284,#11452,#5181,.T.);
#14032=EDGE_CURVE('',#11449,#11453,#5182,.T.);
#14033=EDGE_CURVE('',#11450,#11453,#5183,.T.);
#14034=EDGE_CURVE('',#11454,#11263,#5184,.T.);
#14035=EDGE_CURVE('',#11262,#11455,#5185,.F.);
#14036=EDGE_CURVE('',#11455,#11456,#5186,.T.);
#14037=EDGE_CURVE('',#11456,#11457,#5187,.T.);
#14038=EDGE_CURVE('',#11457,#11454,#5188,.T.);
#14039=EDGE_CURVE('',#11454,#11458,#5189,.T.);
#14040=EDGE_CURVE('',#11459,#11458,#5190,.T.);
#14041=EDGE_CURVE('',#11460,#11459,#5191,.T.);
#14042=EDGE_CURVE('',#11264,#11460,#5192,.T.);
#14043=EDGE_CURVE('',#11457,#11461,#5193,.T.);
#14044=EDGE_CURVE('',#11458,#11461,#5194,.T.);
#14045=EDGE_CURVE('',#11462,#11243,#5195,.T.);
#14046=EDGE_CURVE('',#11242,#11463,#5196,.F.);
#14047=EDGE_CURVE('',#11463,#11464,#5197,.T.);
#14048=EDGE_CURVE('',#11464,#11465,#5198,.T.);
#14049=EDGE_CURVE('',#11465,#11462,#5199,.T.);
#14050=EDGE_CURVE('',#11462,#11466,#5200,.T.);
#14051=EDGE_CURVE('',#11467,#11466,#5201,.T.);
#14052=EDGE_CURVE('',#11468,#11467,#5202,.T.);
#14053=EDGE_CURVE('',#11244,#11468,#5203,.T.);
#14054=EDGE_CURVE('',#11465,#11469,#5204,.T.);
#14055=EDGE_CURVE('',#11466,#11469,#5205,.T.);
#14056=EDGE_CURVE('',#11470,#11223,#5206,.T.);
#14057=EDGE_CURVE('',#11222,#11471,#5207,.F.);
#14058=EDGE_CURVE('',#11471,#11472,#5208,.T.);
#14059=EDGE_CURVE('',#11472,#11473,#5209,.T.);
#14060=EDGE_CURVE('',#11473,#11470,#5210,.T.);
#14061=EDGE_CURVE('',#11470,#11474,#5211,.T.);
#14062=EDGE_CURVE('',#11475,#11474,#5212,.T.);
#14063=EDGE_CURVE('',#11476,#11475,#5213,.T.);
#14064=EDGE_CURVE('',#11224,#11476,#5214,.T.);
#14065=EDGE_CURVE('',#11473,#11477,#5215,.T.);
#14066=EDGE_CURVE('',#11474,#11477,#5216,.T.);
#14067=EDGE_CURVE('',#11478,#11203,#5217,.T.);
#14068=EDGE_CURVE('',#11202,#11479,#5218,.F.);
#14069=EDGE_CURVE('',#11479,#11480,#5219,.T.);
#14070=EDGE_CURVE('',#11480,#11481,#5220,.T.);
#14071=EDGE_CURVE('',#11481,#11478,#5221,.T.);
#14072=EDGE_CURVE('',#11478,#11482,#5222,.T.);
#14073=EDGE_CURVE('',#11483,#11482,#5223,.T.);
#14074=EDGE_CURVE('',#11484,#11483,#5224,.T.);
#14075=EDGE_CURVE('',#11204,#11484,#5225,.T.);
#14076=EDGE_CURVE('',#11481,#11485,#5226,.T.);
#14077=EDGE_CURVE('',#11482,#11485,#5227,.T.);
#14078=EDGE_CURVE('',#11486,#11183,#5228,.T.);
#14079=EDGE_CURVE('',#11182,#11487,#5229,.F.);
#14080=EDGE_CURVE('',#11487,#11488,#5230,.T.);
#14081=EDGE_CURVE('',#11488,#11489,#5231,.T.);
#14082=EDGE_CURVE('',#11489,#11486,#5232,.T.);
#14083=EDGE_CURVE('',#11486,#11490,#5233,.T.);
#14084=EDGE_CURVE('',#11491,#11490,#5234,.T.);
#14085=EDGE_CURVE('',#11492,#11491,#5235,.T.);
#14086=EDGE_CURVE('',#11184,#11492,#5236,.T.);
#14087=EDGE_CURVE('',#11489,#11493,#5237,.T.);
#14088=EDGE_CURVE('',#11490,#11493,#5238,.T.);
#14089=EDGE_CURVE('',#11494,#11495,#5239,.T.);
#14090=EDGE_CURVE('',#11495,#11496,#5240,.T.);
#14091=EDGE_CURVE('',#11496,#11180,#5241,.F.);
#14092=EDGE_CURVE('',#11179,#11497,#5242,.T.);
#14093=EDGE_CURVE('',#11497,#11494,#5243,.T.);
#14094=EDGE_CURVE('',#11495,#11498,#5244,.T.);
#14095=EDGE_CURVE('',#11499,#11498,#5245,.T.);
#14096=EDGE_CURVE('',#11496,#11499,#5246,.T.);
#14097=EDGE_CURVE('',#11494,#11500,#5247,.T.);
#14098=EDGE_CURVE('',#11498,#11500,#5248,.T.);
#14099=EDGE_CURVE('',#11501,#11502,#5249,.T.);
#14100=EDGE_CURVE('',#11502,#11503,#5250,.T.);
#14101=EDGE_CURVE('',#11503,#11400,#5251,.F.);
#14102=EDGE_CURVE('',#11399,#11504,#5252,.T.);
#14103=EDGE_CURVE('',#11504,#11501,#5253,.T.);
#14104=EDGE_CURVE('',#11502,#11505,#5254,.T.);
#14105=EDGE_CURVE('',#11506,#11505,#5255,.T.);
#14106=EDGE_CURVE('',#11503,#11506,#5256,.T.);
#14107=EDGE_CURVE('',#11501,#11507,#5257,.T.);
#14108=EDGE_CURVE('',#11505,#11507,#5258,.T.);
#14109=EDGE_CURVE('',#11508,#11509,#5259,.T.);
#14110=EDGE_CURVE('',#11509,#11510,#5260,.T.);
#14111=EDGE_CURVE('',#11510,#11380,#5261,.F.);
#14112=EDGE_CURVE('',#11379,#11511,#5262,.T.);
#14113=EDGE_CURVE('',#11511,#11508,#5263,.T.);
#14114=EDGE_CURVE('',#11509,#11512,#5264,.T.);
#14115=EDGE_CURVE('',#11513,#11512,#5265,.T.);
#14116=EDGE_CURVE('',#11510,#11513,#5266,.T.);
#14117=EDGE_CURVE('',#11508,#11514,#5267,.T.);
#14118=EDGE_CURVE('',#11512,#11514,#5268,.T.);
#14119=EDGE_CURVE('',#11515,#11516,#5269,.T.);
#14120=EDGE_CURVE('',#11516,#11517,#5270,.T.);
#14121=EDGE_CURVE('',#11517,#11360,#5271,.F.);
#14122=EDGE_CURVE('',#11359,#11518,#5272,.T.);
#14123=EDGE_CURVE('',#11518,#11515,#5273,.T.);
#14124=EDGE_CURVE('',#11516,#11519,#5274,.T.);
#14125=EDGE_CURVE('',#11520,#11519,#5275,.T.);
#14126=EDGE_CURVE('',#11517,#11520,#5276,.T.);
#14127=EDGE_CURVE('',#11515,#11521,#5277,.T.);
#14128=EDGE_CURVE('',#11519,#11521,#5278,.T.);
#14129=EDGE_CURVE('',#11522,#11523,#5279,.T.);
#14130=EDGE_CURVE('',#11523,#11524,#5280,.T.);
#14131=EDGE_CURVE('',#11524,#11340,#5281,.F.);
#14132=EDGE_CURVE('',#11339,#11525,#5282,.T.);
#14133=EDGE_CURVE('',#11525,#11522,#5283,.T.);
#14134=EDGE_CURVE('',#11523,#11526,#5284,.T.);
#14135=EDGE_CURVE('',#11527,#11526,#5285,.T.);
#14136=EDGE_CURVE('',#11524,#11527,#5286,.T.);
#14137=EDGE_CURVE('',#11522,#11528,#5287,.T.);
#14138=EDGE_CURVE('',#11526,#11528,#5288,.T.);
#14139=EDGE_CURVE('',#11529,#11530,#5289,.T.);
#14140=EDGE_CURVE('',#11530,#11531,#5290,.T.);
#14141=EDGE_CURVE('',#11531,#11320,#5291,.F.);
#14142=EDGE_CURVE('',#11319,#11532,#5292,.T.);
#14143=EDGE_CURVE('',#11532,#11529,#5293,.T.);
#14144=EDGE_CURVE('',#11530,#11533,#5294,.T.);
#14145=EDGE_CURVE('',#11534,#11533,#5295,.T.);
#14146=EDGE_CURVE('',#11531,#11534,#5296,.T.);
#14147=EDGE_CURVE('',#11529,#11535,#5297,.T.);
#14148=EDGE_CURVE('',#11533,#11535,#5298,.T.);
#14149=EDGE_CURVE('',#11536,#11537,#5299,.T.);
#14150=EDGE_CURVE('',#11537,#11538,#5300,.T.);
#14151=EDGE_CURVE('',#11538,#11300,#5301,.F.);
#14152=EDGE_CURVE('',#11299,#11539,#5302,.T.);
#14153=EDGE_CURVE('',#11539,#11536,#5303,.T.);
#14154=EDGE_CURVE('',#11537,#11540,#5304,.T.);
#14155=EDGE_CURVE('',#11541,#11540,#5305,.T.);
#14156=EDGE_CURVE('',#11538,#11541,#5306,.T.);
#14157=EDGE_CURVE('',#11536,#11542,#5307,.T.);
#14158=EDGE_CURVE('',#11540,#11542,#5308,.T.);
#14159=EDGE_CURVE('',#11543,#11544,#5309,.T.);
#14160=EDGE_CURVE('',#11544,#11545,#5310,.T.);
#14161=EDGE_CURVE('',#11545,#11280,#5311,.F.);
#14162=EDGE_CURVE('',#11279,#11546,#5312,.T.);
#14163=EDGE_CURVE('',#11546,#11543,#5313,.T.);
#14164=EDGE_CURVE('',#11544,#11547,#5314,.T.);
#14165=EDGE_CURVE('',#11548,#11547,#5315,.T.);
#14166=EDGE_CURVE('',#11545,#11548,#5316,.T.);
#14167=EDGE_CURVE('',#11543,#11549,#5317,.T.);
#14168=EDGE_CURVE('',#11547,#11549,#5318,.T.);
#14169=EDGE_CURVE('',#11550,#11551,#5319,.T.);
#14170=EDGE_CURVE('',#11551,#11552,#5320,.T.);
#14171=EDGE_CURVE('',#11552,#11260,#5321,.F.);
#14172=EDGE_CURVE('',#11259,#11553,#5322,.T.);
#14173=EDGE_CURVE('',#11553,#11550,#5323,.T.);
#14174=EDGE_CURVE('',#11551,#11554,#5324,.T.);
#14175=EDGE_CURVE('',#11555,#11554,#5325,.T.);
#14176=EDGE_CURVE('',#11552,#11555,#5326,.T.);
#14177=EDGE_CURVE('',#11550,#11556,#5327,.T.);
#14178=EDGE_CURVE('',#11554,#11556,#5328,.T.);
#14179=EDGE_CURVE('',#11557,#11558,#5329,.T.);
#14180=EDGE_CURVE('',#11558,#11559,#5330,.T.);
#14181=EDGE_CURVE('',#11559,#11240,#5331,.F.);
#14182=EDGE_CURVE('',#11239,#11560,#5332,.T.);
#14183=EDGE_CURVE('',#11560,#11557,#5333,.T.);
#14184=EDGE_CURVE('',#11558,#11561,#5334,.T.);
#14185=EDGE_CURVE('',#11562,#11561,#5335,.T.);
#14186=EDGE_CURVE('',#11559,#11562,#5336,.T.);
#14187=EDGE_CURVE('',#11557,#11563,#5337,.T.);
#14188=EDGE_CURVE('',#11561,#11563,#5338,.T.);
#14189=EDGE_CURVE('',#11564,#11565,#5339,.T.);
#14190=EDGE_CURVE('',#11565,#11566,#5340,.T.);
#14191=EDGE_CURVE('',#11566,#11220,#5341,.F.);
#14192=EDGE_CURVE('',#11219,#11567,#5342,.T.);
#14193=EDGE_CURVE('',#11567,#11564,#5343,.T.);
#14194=EDGE_CURVE('',#11565,#11568,#5344,.T.);
#14195=EDGE_CURVE('',#11569,#11568,#5345,.T.);
#14196=EDGE_CURVE('',#11566,#11569,#5346,.T.);
#14197=EDGE_CURVE('',#11564,#11570,#5347,.T.);
#14198=EDGE_CURVE('',#11568,#11570,#5348,.T.);
#14199=EDGE_CURVE('',#11571,#11572,#5349,.T.);
#14200=EDGE_CURVE('',#11572,#11573,#5350,.T.);
#14201=EDGE_CURVE('',#11573,#11200,#5351,.F.);
#14202=EDGE_CURVE('',#11199,#11574,#5352,.T.);
#14203=EDGE_CURVE('',#11574,#11571,#5353,.T.);
#14204=EDGE_CURVE('',#11572,#11575,#5354,.T.);
#14205=EDGE_CURVE('',#11576,#11575,#5355,.T.);
#14206=EDGE_CURVE('',#11573,#11576,#5356,.T.);
#14207=EDGE_CURVE('',#11571,#11577,#5357,.T.);
#14208=EDGE_CURVE('',#11575,#11577,#5358,.T.);
#14209=EDGE_CURVE('',#11493,#11578,#5359,.T.);
#14210=EDGE_CURVE('',#11578,#11579,#5360,.T.);
#14211=EDGE_CURVE('',#11579,#11580,#5361,.F.);
#14212=EDGE_CURVE('',#11580,#11491,#5362,.T.);
#14213=EDGE_CURVE('',#11580,#11581,#5363,.T.);
#14214=EDGE_CURVE('',#11581,#11582,#5364,.T.);
#14215=EDGE_CURVE('',#11583,#11582,#5365,.T.);
#14216=EDGE_CURVE('',#11583,#11584,#5366,.T.);
#14217=EDGE_CURVE('',#11584,#11585,#5367,.T.);
#14218=EDGE_CURVE('',#11585,#11586,#5368,.T.);
#14219=EDGE_CURVE('',#11586,#11587,#5369,.T.);
#14220=EDGE_CURVE('',#11587,#11588,#5370,.T.);
#14221=EDGE_CURVE('',#11588,#11589,#5371,.T.);
#14222=EDGE_CURVE('',#11589,#11590,#5372,.T.);
#14223=EDGE_CURVE('',#11590,#11591,#5373,.T.);
#14224=EDGE_CURVE('',#11591,#11592,#5374,.T.);
#14225=EDGE_CURVE('',#11592,#11593,#5375,.T.);
#14226=EDGE_CURVE('',#11593,#11594,#5376,.T.);
#14227=EDGE_CURVE('',#11594,#11595,#5377,.T.);
#14228=EDGE_CURVE('',#11595,#11596,#5378,.T.);
#14229=EDGE_CURVE('',#11596,#11597,#5379,.T.);
#14230=EDGE_CURVE('',#11597,#11404,#5380,.T.);
#14231=EDGE_CURVE('',#11598,#11403,#5381,.T.);
#14232=EDGE_CURVE('',#11598,#11599,#5382,.T.);
#14233=EDGE_CURVE('',#11599,#11600,#5383,.T.);
#14234=EDGE_CURVE('',#11601,#11600,#5384,.T.);
#14235=EDGE_CURVE('',#11601,#11602,#5385,.T.);
#14236=EDGE_CURVE('',#11602,#11603,#5386,.T.);
#14237=EDGE_CURVE('',#11603,#11604,#5387,.T.);
#14238=EDGE_CURVE('',#11604,#11605,#5388,.T.);
#14239=EDGE_CURVE('',#11605,#11606,#5389,.T.);
#14240=EDGE_CURVE('',#11606,#11607,#5390,.T.);
#14241=EDGE_CURVE('',#11607,#11608,#5391,.T.);
#14242=EDGE_CURVE('',#11608,#11609,#5392,.T.);
#14243=EDGE_CURVE('',#11609,#11610,#5393,.T.);
#14244=EDGE_CURVE('',#11610,#11611,#5394,.T.);
#14245=EDGE_CURVE('',#11611,#11612,#5395,.T.);
#14246=EDGE_CURVE('',#11612,#11613,#5396,.T.);
#14247=EDGE_CURVE('',#11613,#11614,#5397,.T.);
#14248=EDGE_CURVE('',#11614,#11615,#5398,.T.);
#14249=EDGE_CURVE('',#11615,#11412,#5399,.T.);
#14250=EDGE_CURVE('',#11616,#11411,#5400,.T.);
#14251=EDGE_CURVE('',#11616,#11617,#5401,.T.);
#14252=EDGE_CURVE('',#11617,#11618,#5402,.T.);
#14253=EDGE_CURVE('',#11619,#11618,#5403,.T.);
#14254=EDGE_CURVE('',#11619,#11620,#5404,.T.);
#14255=EDGE_CURVE('',#11620,#11621,#5405,.T.);
#14256=EDGE_CURVE('',#11621,#11622,#5406,.T.);
#14257=EDGE_CURVE('',#11622,#11623,#5407,.T.);
#14258=EDGE_CURVE('',#11623,#11624,#5408,.T.);
#14259=EDGE_CURVE('',#11624,#11625,#5409,.T.);
#14260=EDGE_CURVE('',#11625,#11626,#5410,.T.);
#14261=EDGE_CURVE('',#11626,#11627,#5411,.T.);
#14262=EDGE_CURVE('',#11627,#11628,#5412,.T.);
#14263=EDGE_CURVE('',#11628,#11629,#5413,.T.);
#14264=EDGE_CURVE('',#11629,#11630,#5414,.T.);
#14265=EDGE_CURVE('',#11630,#11631,#5415,.T.);
#14266=EDGE_CURVE('',#11631,#11632,#5416,.T.);
#14267=EDGE_CURVE('',#11632,#11633,#5417,.T.);
#14268=EDGE_CURVE('',#11633,#11420,#5418,.T.);
#14269=EDGE_CURVE('',#11634,#11419,#5419,.T.);
#14270=EDGE_CURVE('',#11634,#11635,#5420,.T.);
#14271=EDGE_CURVE('',#11635,#11636,#5421,.T.);
#14272=EDGE_CURVE('',#11637,#11636,#5422,.T.);
#14273=EDGE_CURVE('',#11637,#11638,#5423,.T.);
#14274=EDGE_CURVE('',#11638,#11639,#5424,.T.);
#14275=EDGE_CURVE('',#11639,#11640,#5425,.T.);
#14276=EDGE_CURVE('',#11640,#11641,#5426,.T.);
#14277=EDGE_CURVE('',#11641,#11642,#5427,.T.);
#14278=EDGE_CURVE('',#11642,#11643,#5428,.T.);
#14279=EDGE_CURVE('',#11643,#11644,#5429,.T.);
#14280=EDGE_CURVE('',#11644,#11645,#5430,.T.);
#14281=EDGE_CURVE('',#11645,#11646,#5431,.T.);
#14282=EDGE_CURVE('',#11646,#11647,#5432,.T.);
#14283=EDGE_CURVE('',#11647,#11648,#5433,.T.);
#14284=EDGE_CURVE('',#11648,#11649,#5434,.T.);
#14285=EDGE_CURVE('',#11649,#11650,#5435,.T.);
#14286=EDGE_CURVE('',#11650,#11651,#5436,.T.);
#14287=EDGE_CURVE('',#11651,#11428,#5437,.T.);
#14288=EDGE_CURVE('',#11652,#11427,#5438,.T.);
#14289=EDGE_CURVE('',#11652,#11653,#5439,.T.);
#14290=EDGE_CURVE('',#11653,#11654,#5440,.T.);
#14291=EDGE_CURVE('',#11655,#11654,#5441,.T.);
#14292=EDGE_CURVE('',#11655,#11656,#5442,.T.);
#14293=EDGE_CURVE('',#11656,#11657,#5443,.T.);
#14294=EDGE_CURVE('',#11657,#11658,#5444,.T.);
#14295=EDGE_CURVE('',#11658,#11659,#5445,.T.);
#14296=EDGE_CURVE('',#11659,#11660,#5446,.T.);
#14297=EDGE_CURVE('',#11660,#11661,#5447,.T.);
#14298=EDGE_CURVE('',#11661,#11662,#5448,.T.);
#14299=EDGE_CURVE('',#11662,#11663,#5449,.T.);
#14300=EDGE_CURVE('',#11663,#11664,#5450,.T.);
#14301=EDGE_CURVE('',#11664,#11665,#5451,.T.);
#14302=EDGE_CURVE('',#11665,#11666,#5452,.T.);
#14303=EDGE_CURVE('',#11666,#11667,#5453,.T.);
#14304=EDGE_CURVE('',#11667,#11668,#5454,.T.);
#14305=EDGE_CURVE('',#11668,#11669,#5455,.T.);
#14306=EDGE_CURVE('',#11669,#11436,#5456,.T.);
#14307=EDGE_CURVE('',#11670,#11435,#5457,.T.);
#14308=EDGE_CURVE('',#11670,#11671,#5458,.T.);
#14309=EDGE_CURVE('',#11671,#11672,#5459,.T.);
#14310=EDGE_CURVE('',#11673,#11672,#5460,.T.);
#14311=EDGE_CURVE('',#11673,#11674,#5461,.T.);
#14312=EDGE_CURVE('',#11674,#11675,#5462,.T.);
#14313=EDGE_CURVE('',#11675,#11676,#5463,.T.);
#14314=EDGE_CURVE('',#11676,#11677,#5464,.T.);
#14315=EDGE_CURVE('',#11677,#11678,#5465,.T.);
#14316=EDGE_CURVE('',#11678,#11679,#5466,.T.);
#14317=EDGE_CURVE('',#11679,#11680,#5467,.T.);
#14318=EDGE_CURVE('',#11680,#11681,#5468,.T.);
#14319=EDGE_CURVE('',#11681,#11682,#5469,.T.);
#14320=EDGE_CURVE('',#11682,#11683,#5470,.T.);
#14321=EDGE_CURVE('',#11683,#11684,#5471,.T.);
#14322=EDGE_CURVE('',#11684,#11685,#5472,.T.);
#14323=EDGE_CURVE('',#11685,#11686,#5473,.T.);
#14324=EDGE_CURVE('',#11686,#11687,#5474,.T.);
#14325=EDGE_CURVE('',#11687,#11444,#5475,.T.);
#14326=EDGE_CURVE('',#11688,#11443,#5476,.T.);
#14327=EDGE_CURVE('',#11688,#11689,#5477,.T.);
#14328=EDGE_CURVE('',#11689,#11690,#5478,.T.);
#14329=EDGE_CURVE('',#11691,#11690,#5479,.T.);
#14330=EDGE_CURVE('',#11691,#11692,#5480,.T.);
#14331=EDGE_CURVE('',#11692,#11693,#5481,.T.);
#14332=EDGE_CURVE('',#11693,#11694,#5482,.T.);
#14333=EDGE_CURVE('',#11694,#11695,#5483,.T.);
#14334=EDGE_CURVE('',#11695,#11696,#5484,.T.);
#14335=EDGE_CURVE('',#11696,#11697,#5485,.T.);
#14336=EDGE_CURVE('',#11697,#11698,#5486,.T.);
#14337=EDGE_CURVE('',#11698,#11699,#5487,.T.);
#14338=EDGE_CURVE('',#11699,#11700,#5488,.T.);
#14339=EDGE_CURVE('',#11700,#11701,#5489,.T.);
#14340=EDGE_CURVE('',#11701,#11702,#5490,.T.);
#14341=EDGE_CURVE('',#11702,#11703,#5491,.T.);
#14342=EDGE_CURVE('',#11703,#11704,#5492,.T.);
#14343=EDGE_CURVE('',#11704,#11705,#5493,.T.);
#14344=EDGE_CURVE('',#11705,#11452,#5494,.T.);
#14345=EDGE_CURVE('',#11706,#11451,#5495,.T.);
#14346=EDGE_CURVE('',#11706,#11707,#5496,.T.);
#14347=EDGE_CURVE('',#11707,#11708,#5497,.T.);
#14348=EDGE_CURVE('',#11709,#11708,#5498,.T.);
#14349=EDGE_CURVE('',#11709,#11710,#5499,.T.);
#14350=EDGE_CURVE('',#11710,#11711,#5500,.T.);
#14351=EDGE_CURVE('',#11711,#11712,#5501,.T.);
#14352=EDGE_CURVE('',#11712,#11713,#5502,.T.);
#14353=EDGE_CURVE('',#11713,#11714,#5503,.T.);
#14354=EDGE_CURVE('',#11714,#11715,#5504,.T.);
#14355=EDGE_CURVE('',#11715,#11716,#5505,.T.);
#14356=EDGE_CURVE('',#11716,#11717,#5506,.T.);
#14357=EDGE_CURVE('',#11717,#11718,#5507,.T.);
#14358=EDGE_CURVE('',#11718,#11719,#5508,.T.);
#14359=EDGE_CURVE('',#11719,#11720,#5509,.T.);
#14360=EDGE_CURVE('',#11720,#11721,#5510,.T.);
#14361=EDGE_CURVE('',#11721,#11722,#5511,.T.);
#14362=EDGE_CURVE('',#11722,#11723,#5512,.T.);
#14363=EDGE_CURVE('',#11723,#11460,#5513,.T.);
#14364=EDGE_CURVE('',#11724,#11459,#5514,.T.);
#14365=EDGE_CURVE('',#11724,#11725,#5515,.T.);
#14366=EDGE_CURVE('',#11725,#11726,#5516,.T.);
#14367=EDGE_CURVE('',#11727,#11726,#5517,.T.);
#14368=EDGE_CURVE('',#11727,#11728,#5518,.T.);
#14369=EDGE_CURVE('',#11728,#11729,#5519,.T.);
#14370=EDGE_CURVE('',#11729,#11730,#5520,.T.);
#14371=EDGE_CURVE('',#11730,#11731,#5521,.T.);
#14372=EDGE_CURVE('',#11731,#11732,#5522,.T.);
#14373=EDGE_CURVE('',#11732,#11733,#5523,.T.);
#14374=EDGE_CURVE('',#11733,#11734,#5524,.T.);
#14375=EDGE_CURVE('',#11734,#11735,#5525,.T.);
#14376=EDGE_CURVE('',#11735,#11736,#5526,.T.);
#14377=EDGE_CURVE('',#11736,#11737,#5527,.T.);
#14378=EDGE_CURVE('',#11737,#11738,#5528,.T.);
#14379=EDGE_CURVE('',#11738,#11739,#5529,.T.);
#14380=EDGE_CURVE('',#11739,#11740,#5530,.T.);
#14381=EDGE_CURVE('',#11740,#11741,#5531,.T.);
#14382=EDGE_CURVE('',#11741,#11468,#5532,.T.);
#14383=EDGE_CURVE('',#11742,#11467,#5533,.T.);
#14384=EDGE_CURVE('',#11742,#11743,#5534,.T.);
#14385=EDGE_CURVE('',#11743,#11744,#5535,.T.);
#14386=EDGE_CURVE('',#11745,#11744,#5536,.T.);
#14387=EDGE_CURVE('',#11745,#11746,#5537,.T.);
#14388=EDGE_CURVE('',#11746,#11747,#5538,.T.);
#14389=EDGE_CURVE('',#11747,#11748,#5539,.T.);
#14390=EDGE_CURVE('',#11748,#11749,#5540,.T.);
#14391=EDGE_CURVE('',#11749,#11750,#5541,.T.);
#14392=EDGE_CURVE('',#11750,#11751,#5542,.T.);
#14393=EDGE_CURVE('',#11751,#11752,#5543,.T.);
#14394=EDGE_CURVE('',#11752,#11753,#5544,.T.);
#14395=EDGE_CURVE('',#11753,#11754,#5545,.T.);
#14396=EDGE_CURVE('',#11754,#11755,#5546,.T.);
#14397=EDGE_CURVE('',#11755,#11756,#5547,.T.);
#14398=EDGE_CURVE('',#11756,#11757,#5548,.T.);
#14399=EDGE_CURVE('',#11757,#11758,#5549,.T.);
#14400=EDGE_CURVE('',#11758,#11759,#5550,.T.);
#14401=EDGE_CURVE('',#11759,#11476,#5551,.T.);
#14402=EDGE_CURVE('',#11760,#11475,#5552,.T.);
#14403=EDGE_CURVE('',#11760,#11761,#5553,.T.);
#14404=EDGE_CURVE('',#11761,#11762,#5554,.T.);
#14405=EDGE_CURVE('',#11763,#11762,#5555,.T.);
#14406=EDGE_CURVE('',#11763,#11764,#5556,.T.);
#14407=EDGE_CURVE('',#11764,#11765,#5557,.T.);
#14408=EDGE_CURVE('',#11765,#11766,#5558,.T.);
#14409=EDGE_CURVE('',#11766,#11767,#5559,.T.);
#14410=EDGE_CURVE('',#11767,#11768,#5560,.T.);
#14411=EDGE_CURVE('',#11768,#11769,#5561,.T.);
#14412=EDGE_CURVE('',#11769,#11770,#5562,.T.);
#14413=EDGE_CURVE('',#11770,#11771,#5563,.T.);
#14414=EDGE_CURVE('',#11771,#11772,#5564,.T.);
#14415=EDGE_CURVE('',#11772,#11773,#5565,.T.);
#14416=EDGE_CURVE('',#11773,#11774,#5566,.T.);
#14417=EDGE_CURVE('',#11774,#11775,#5567,.T.);
#14418=EDGE_CURVE('',#11775,#11776,#5568,.T.);
#14419=EDGE_CURVE('',#11776,#11777,#5569,.T.);
#14420=EDGE_CURVE('',#11777,#11484,#5570,.T.);
#14421=EDGE_CURVE('',#11778,#11483,#5571,.T.);
#14422=EDGE_CURVE('',#11778,#11779,#5572,.T.);
#14423=EDGE_CURVE('',#11779,#11780,#5573,.T.);
#14424=EDGE_CURVE('',#11781,#11780,#5574,.T.);
#14425=EDGE_CURVE('',#11781,#11782,#5575,.T.);
#14426=EDGE_CURVE('',#11782,#11783,#5576,.T.);
#14427=EDGE_CURVE('',#11783,#11784,#5577,.T.);
#14428=EDGE_CURVE('',#11784,#11785,#5578,.T.);
#14429=EDGE_CURVE('',#11785,#11786,#5579,.T.);
#14430=EDGE_CURVE('',#11786,#11787,#5580,.T.);
#14431=EDGE_CURVE('',#11787,#11788,#5581,.T.);
#14432=EDGE_CURVE('',#11788,#11789,#5582,.T.);
#14433=EDGE_CURVE('',#11789,#11790,#5583,.T.);
#14434=EDGE_CURVE('',#11790,#11791,#5584,.T.);
#14435=EDGE_CURVE('',#11791,#11792,#5585,.T.);
#14436=EDGE_CURVE('',#11792,#11793,#5586,.T.);
#14437=EDGE_CURVE('',#11793,#11794,#5587,.T.);
#14438=EDGE_CURVE('',#11794,#11795,#5588,.T.);
#14439=EDGE_CURVE('',#11795,#11492,#5589,.T.);
#14440=EDGE_CURVE('',#11796,#11796,#10569,.T.);
#14441=EDGE_CURVE('',#11797,#11781,#5590,.T.);
#14442=EDGE_CURVE('',#11780,#11576,#5591,.F.);
#14443=EDGE_CURVE('',#11577,#11797,#5592,.T.);
#14444=EDGE_CURVE('',#11485,#11798,#5593,.T.);
#14445=EDGE_CURVE('',#11798,#11799,#5594,.T.);
#14446=EDGE_CURVE('',#11799,#11778,#5595,.F.);
#14447=EDGE_CURVE('',#11800,#11763,#5596,.T.);
#14448=EDGE_CURVE('',#11762,#11569,#5597,.F.);
#14449=EDGE_CURVE('',#11570,#11800,#5598,.T.);
#14450=EDGE_CURVE('',#11477,#11801,#5599,.T.);
#14451=EDGE_CURVE('',#11801,#11802,#5600,.T.);
#14452=EDGE_CURVE('',#11802,#11760,#5601,.F.);
#14453=EDGE_CURVE('',#11803,#11745,#5602,.T.);
#14454=EDGE_CURVE('',#11744,#11562,#5603,.F.);
#14455=EDGE_CURVE('',#11563,#11803,#5604,.T.);
#14456=EDGE_CURVE('',#11469,#11804,#5605,.T.);
#14457=EDGE_CURVE('',#11804,#11805,#5606,.T.);
#14458=EDGE_CURVE('',#11805,#11742,#5607,.F.);
#14459=EDGE_CURVE('',#11806,#11727,#5608,.T.);
#14460=EDGE_CURVE('',#11726,#11555,#5609,.F.);
#14461=EDGE_CURVE('',#11556,#11806,#5610,.T.);
#14462=EDGE_CURVE('',#11461,#11807,#5611,.T.);
#14463=EDGE_CURVE('',#11807,#11808,#5612,.T.);
#14464=EDGE_CURVE('',#11808,#11724,#5613,.F.);
#14465=EDGE_CURVE('',#11809,#11709,#5614,.T.);
#14466=EDGE_CURVE('',#11708,#11548,#5615,.F.);
#14467=EDGE_CURVE('',#11549,#11809,#5616,.T.);
#14468=EDGE_CURVE('',#11453,#11810,#5617,.T.);
#14469=EDGE_CURVE('',#11810,#11811,#5618,.T.);
#14470=EDGE_CURVE('',#11811,#11706,#5619,.F.);
#14471=EDGE_CURVE('',#11812,#11691,#5620,.T.);
#14472=EDGE_CURVE('',#11690,#11541,#5621,.F.);
#14473=EDGE_CURVE('',#11542,#11812,#5622,.T.);
#14474=EDGE_CURVE('',#11445,#11813,#5623,.T.);
#14475=EDGE_CURVE('',#11813,#11814,#5624,.T.);
#14476=EDGE_CURVE('',#11814,#11688,#5625,.F.);
#14477=EDGE_CURVE('',#11815,#11673,#5626,.T.);
#14478=EDGE_CURVE('',#11672,#11534,#5627,.F.);
#14479=EDGE_CURVE('',#11535,#11815,#5628,.T.);
#14480=EDGE_CURVE('',#11437,#11816,#5629,.T.);
#14481=EDGE_CURVE('',#11816,#11817,#5630,.T.);
#14482=EDGE_CURVE('',#11817,#11670,#5631,.F.);
#14483=EDGE_CURVE('',#11818,#11655,#5632,.T.);
#14484=EDGE_CURVE('',#11654,#11527,#5633,.F.);
#14485=EDGE_CURVE('',#11528,#11818,#5634,.T.);
#14486=EDGE_CURVE('',#11429,#11819,#5635,.T.);
#14487=EDGE_CURVE('',#11819,#11820,#5636,.T.);
#14488=EDGE_CURVE('',#11820,#11652,#5637,.F.);
#14489=EDGE_CURVE('',#11821,#11637,#5638,.T.);
#14490=EDGE_CURVE('',#11636,#11520,#5639,.F.);
#14491=EDGE_CURVE('',#11521,#11821,#5640,.T.);
#14492=EDGE_CURVE('',#11421,#11822,#5641,.T.);
#14493=EDGE_CURVE('',#11822,#11823,#5642,.T.);
#14494=EDGE_CURVE('',#11823,#11634,#5643,.F.);
#14495=EDGE_CURVE('',#11824,#11619,#5644,.T.);
#14496=EDGE_CURVE('',#11618,#11513,#5645,.F.);
#14497=EDGE_CURVE('',#11514,#11824,#5646,.T.);
#14498=EDGE_CURVE('',#11413,#11825,#5647,.T.);
#14499=EDGE_CURVE('',#11825,#11826,#5648,.T.);
#14500=EDGE_CURVE('',#11826,#11616,#5649,.F.);
#14501=EDGE_CURVE('',#11827,#11601,#5650,.T.);
#14502=EDGE_CURVE('',#11600,#11506,#5651,.F.);
#14503=EDGE_CURVE('',#11507,#11827,#5652,.T.);
#14504=EDGE_CURVE('',#11405,#11828,#5653,.T.);
#14505=EDGE_CURVE('',#11828,#11829,#5654,.T.);
#14506=EDGE_CURVE('',#11829,#11598,#5655,.F.);
#14507=EDGE_CURVE('',#11830,#11583,#5656,.T.);
#14508=EDGE_CURVE('',#11582,#11499,#5657,.F.);
#14509=EDGE_CURVE('',#11500,#11830,#5658,.T.);
#14510=EDGE_CURVE('',#11831,#11832,#10570,.T.);
#14511=EDGE_CURVE('',#11831,#11833,#5659,.T.);
#14512=EDGE_CURVE('',#11833,#11834,#5660,.T.);
#14513=EDGE_CURVE('',#11832,#11834,#5661,.T.);
#14514=EDGE_CURVE('',#11832,#11835,#5662,.T.);
#14515=EDGE_CURVE('',#11834,#11836,#5663,.T.);
#14516=EDGE_CURVE('',#11835,#11836,#5664,.T.);
#14517=EDGE_CURVE('',#11837,#11831,#5665,.T.);
#14518=EDGE_CURVE('',#11837,#11838,#5666,.T.);
#14519=EDGE_CURVE('',#11838,#11833,#5667,.T.);
#14520=EDGE_CURVE('',#11835,#11837,#10571,.T.);
#14521=EDGE_CURVE('',#11836,#11838,#5668,.T.);
#14522=EDGE_CURVE('',#11181,#11581,#5669,.T.);
#14523=EDGE_CURVE('',#11487,#11579,#5670,.T.);
#14524=EDGE_CURVE('',#11488,#11578,#5671,.T.);
#14525=EDGE_CURVE('',#11185,#11795,#5672,.T.);
#14526=EDGE_CURVE('',#11186,#11794,#5673,.T.);
#14527=EDGE_CURVE('',#11187,#11793,#5674,.T.);
#14528=EDGE_CURVE('',#11188,#11792,#5675,.T.);
#14529=EDGE_CURVE('',#11189,#11791,#5676,.T.);
#14530=EDGE_CURVE('',#11190,#11790,#5677,.T.);
#14531=EDGE_CURVE('',#11191,#11789,#5678,.T.);
#14532=EDGE_CURVE('',#11192,#11788,#5679,.T.);
#14533=EDGE_CURVE('',#11193,#11787,#5680,.T.);
#14534=EDGE_CURVE('',#11194,#11786,#5681,.T.);
#14535=EDGE_CURVE('',#11195,#11785,#5682,.T.);
#14536=EDGE_CURVE('',#11196,#11784,#5683,.T.);
#14537=EDGE_CURVE('',#11197,#11783,#5684,.T.);
#14538=EDGE_CURVE('',#11198,#11782,#5685,.T.);
#14539=EDGE_CURVE('',#11574,#11797,#5686,.T.);
#14540=EDGE_CURVE('',#11201,#11779,#5687,.T.);
#14541=EDGE_CURVE('',#11479,#11799,#5688,.T.);
#14542=EDGE_CURVE('',#11480,#11798,#5689,.T.);
#14543=EDGE_CURVE('',#11205,#11777,#5690,.T.);
#14544=EDGE_CURVE('',#11206,#11776,#5691,.T.);
#14545=EDGE_CURVE('',#11207,#11775,#5692,.T.);
#14546=EDGE_CURVE('',#11208,#11774,#5693,.T.);
#14547=EDGE_CURVE('',#11209,#11773,#5694,.T.);
#14548=EDGE_CURVE('',#11210,#11772,#5695,.T.);
#14549=EDGE_CURVE('',#11211,#11771,#5696,.T.);
#14550=EDGE_CURVE('',#11212,#11770,#5697,.T.);
#14551=EDGE_CURVE('',#11213,#11769,#5698,.T.);
#14552=EDGE_CURVE('',#11214,#11768,#5699,.T.);
#14553=EDGE_CURVE('',#11215,#11767,#5700,.T.);
#14554=EDGE_CURVE('',#11216,#11766,#5701,.T.);
#14555=EDGE_CURVE('',#11217,#11765,#5702,.T.);
#14556=EDGE_CURVE('',#11218,#11764,#5703,.T.);
#14557=EDGE_CURVE('',#11567,#11800,#5704,.T.);
#14558=EDGE_CURVE('',#11221,#11761,#5705,.T.);
#14559=EDGE_CURVE('',#11471,#11802,#5706,.T.);
#14560=EDGE_CURVE('',#11472,#11801,#5707,.T.);
#14561=EDGE_CURVE('',#11225,#11759,#5708,.T.);
#14562=EDGE_CURVE('',#11226,#11758,#5709,.T.);
#14563=EDGE_CURVE('',#11227,#11757,#5710,.T.);
#14564=EDGE_CURVE('',#11228,#11756,#5711,.T.);
#14565=EDGE_CURVE('',#11229,#11755,#5712,.T.);
#14566=EDGE_CURVE('',#11230,#11754,#5713,.T.);
#14567=EDGE_CURVE('',#11231,#11753,#5714,.T.);
#14568=EDGE_CURVE('',#11232,#11752,#5715,.T.);
#14569=EDGE_CURVE('',#11233,#11751,#5716,.T.);
#14570=EDGE_CURVE('',#11234,#11750,#5717,.T.);
#14571=EDGE_CURVE('',#11235,#11749,#5718,.T.);
#14572=EDGE_CURVE('',#11236,#11748,#5719,.T.);
#14573=EDGE_CURVE('',#11237,#11747,#5720,.T.);
#14574=EDGE_CURVE('',#11238,#11746,#5721,.T.);
#14575=EDGE_CURVE('',#11560,#11803,#5722,.T.);
#14576=EDGE_CURVE('',#11241,#11743,#5723,.T.);
#14577=EDGE_CURVE('',#11463,#11805,#5724,.T.);
#14578=EDGE_CURVE('',#11464,#11804,#5725,.T.);
#14579=EDGE_CURVE('',#11245,#11741,#5726,.T.);
#14580=EDGE_CURVE('',#11246,#11740,#5727,.T.);
#14581=EDGE_CURVE('',#11247,#11739,#5728,.T.);
#14582=EDGE_CURVE('',#11248,#11738,#5729,.T.);
#14583=EDGE_CURVE('',#11249,#11737,#5730,.T.);
#14584=EDGE_CURVE('',#11250,#11736,#5731,.T.);
#14585=EDGE_CURVE('',#11251,#11735,#5732,.T.);
#14586=EDGE_CURVE('',#11252,#11734,#5733,.T.);
#14587=EDGE_CURVE('',#11253,#11733,#5734,.T.);
#14588=EDGE_CURVE('',#11254,#11732,#5735,.T.);
#14589=EDGE_CURVE('',#11255,#11731,#5736,.T.);
#14590=EDGE_CURVE('',#11256,#11730,#5737,.T.);
#14591=EDGE_CURVE('',#11257,#11729,#5738,.T.);
#14592=EDGE_CURVE('',#11258,#11728,#5739,.T.);
#14593=EDGE_CURVE('',#11553,#11806,#5740,.T.);
#14594=EDGE_CURVE('',#11261,#11725,#5741,.T.);
#14595=EDGE_CURVE('',#11455,#11808,#5742,.T.);
#14596=EDGE_CURVE('',#11456,#11807,#5743,.T.);
#14597=EDGE_CURVE('',#11265,#11723,#5744,.T.);
#14598=EDGE_CURVE('',#11266,#11722,#5745,.T.);
#14599=EDGE_CURVE('',#11267,#11721,#5746,.T.);
#14600=EDGE_CURVE('',#11268,#11720,#5747,.T.);
#14601=EDGE_CURVE('',#11269,#11719,#5748,.T.);
#14602=EDGE_CURVE('',#11270,#11718,#5749,.T.);
#14603=EDGE_CURVE('',#11271,#11717,#5750,.T.);
#14604=EDGE_CURVE('',#11272,#11716,#5751,.T.);
#14605=EDGE_CURVE('',#11273,#11715,#5752,.T.);
#14606=EDGE_CURVE('',#11274,#11714,#5753,.T.);
#14607=EDGE_CURVE('',#11275,#11713,#5754,.T.);
#14608=EDGE_CURVE('',#11276,#11712,#5755,.T.);
#14609=EDGE_CURVE('',#11277,#11711,#5756,.T.);
#14610=EDGE_CURVE('',#11278,#11710,#5757,.T.);
#14611=EDGE_CURVE('',#11546,#11809,#5758,.T.);
#14612=EDGE_CURVE('',#11281,#11707,#5759,.T.);
#14613=EDGE_CURVE('',#11447,#11811,#5760,.T.);
#14614=EDGE_CURVE('',#11448,#11810,#5761,.T.);
#14615=EDGE_CURVE('',#11285,#11705,#5762,.T.);
#14616=EDGE_CURVE('',#11286,#11704,#5763,.T.);
#14617=EDGE_CURVE('',#11287,#11703,#5764,.T.);
#14618=EDGE_CURVE('',#11288,#11702,#5765,.T.);
#14619=EDGE_CURVE('',#11289,#11701,#5766,.T.);
#14620=EDGE_CURVE('',#11290,#11700,#5767,.T.);
#14621=EDGE_CURVE('',#11291,#11699,#5768,.T.);
#14622=EDGE_CURVE('',#11292,#11698,#5769,.T.);
#14623=EDGE_CURVE('',#11293,#11697,#5770,.T.);
#14624=EDGE_CURVE('',#11294,#11696,#5771,.T.);
#14625=EDGE_CURVE('',#11295,#11695,#5772,.T.);
#14626=EDGE_CURVE('',#11296,#11694,#5773,.T.);
#14627=EDGE_CURVE('',#11297,#11693,#5774,.T.);
#14628=EDGE_CURVE('',#11298,#11692,#5775,.T.);
#14629=EDGE_CURVE('',#11539,#11812,#5776,.T.);
#14630=EDGE_CURVE('',#11301,#11689,#5777,.T.);
#14631=EDGE_CURVE('',#11439,#11814,#5778,.T.);
#14632=EDGE_CURVE('',#11440,#11813,#5779,.T.);
#14633=EDGE_CURVE('',#11305,#11687,#5780,.T.);
#14634=EDGE_CURVE('',#11306,#11686,#5781,.T.);
#14635=EDGE_CURVE('',#11307,#11685,#5782,.T.);
#14636=EDGE_CURVE('',#11308,#11684,#5783,.T.);
#14637=EDGE_CURVE('',#11309,#11683,#5784,.T.);
#14638=EDGE_CURVE('',#11310,#11682,#5785,.T.);
#14639=EDGE_CURVE('',#11311,#11681,#5786,.T.);
#14640=EDGE_CURVE('',#11312,#11680,#5787,.T.);
#14641=EDGE_CURVE('',#11313,#11679,#5788,.T.);
#14642=EDGE_CURVE('',#11314,#11678,#5789,.T.);
#14643=EDGE_CURVE('',#11315,#11677,#5790,.T.);
#14644=EDGE_CURVE('',#11316,#11676,#5791,.T.);
#14645=EDGE_CURVE('',#11317,#11675,#5792,.T.);
#14646=EDGE_CURVE('',#11318,#11674,#5793,.T.);
#14647=EDGE_CURVE('',#11532,#11815,#5794,.T.);
#14648=EDGE_CURVE('',#11321,#11671,#5795,.T.);
#14649=EDGE_CURVE('',#11431,#11817,#5796,.T.);
#14650=EDGE_CURVE('',#11432,#11816,#5797,.T.);
#14651=EDGE_CURVE('',#11325,#11669,#5798,.T.);
#14652=EDGE_CURVE('',#11326,#11668,#5799,.T.);
#14653=EDGE_CURVE('',#11327,#11667,#5800,.T.);
#14654=EDGE_CURVE('',#11328,#11666,#5801,.T.);
#14655=EDGE_CURVE('',#11329,#11665,#5802,.T.);
#14656=EDGE_CURVE('',#11330,#11664,#5803,.T.);
#14657=EDGE_CURVE('',#11331,#11663,#5804,.T.);
#14658=EDGE_CURVE('',#11332,#11662,#5805,.T.);
#14659=EDGE_CURVE('',#11333,#11661,#5806,.T.);
#14660=EDGE_CURVE('',#11334,#11660,#5807,.T.);
#14661=EDGE_CURVE('',#11335,#11659,#5808,.T.);
#14662=EDGE_CURVE('',#11336,#11658,#5809,.T.);
#14663=EDGE_CURVE('',#11337,#11657,#5810,.T.);
#14664=EDGE_CURVE('',#11338,#11656,#5811,.T.);
#14665=EDGE_CURVE('',#11525,#11818,#5812,.T.);
#14666=EDGE_CURVE('',#11341,#11653,#5813,.T.);
#14667=EDGE_CURVE('',#11423,#11820,#5814,.T.);
#14668=EDGE_CURVE('',#11424,#11819,#5815,.T.);
#14669=EDGE_CURVE('',#11345,#11651,#5816,.T.);
#14670=EDGE_CURVE('',#11346,#11650,#5817,.T.);
#14671=EDGE_CURVE('',#11347,#11649,#5818,.T.);
#14672=EDGE_CURVE('',#11348,#11648,#5819,.T.);
#14673=EDGE_CURVE('',#11349,#11647,#5820,.T.);
#14674=EDGE_CURVE('',#11350,#11646,#5821,.T.);
#14675=EDGE_CURVE('',#11351,#11645,#5822,.T.);
#14676=EDGE_CURVE('',#11352,#11644,#5823,.T.);
#14677=EDGE_CURVE('',#11353,#11643,#5824,.T.);
#14678=EDGE_CURVE('',#11354,#11642,#5825,.T.);
#14679=EDGE_CURVE('',#11355,#11641,#5826,.T.);
#14680=EDGE_CURVE('',#11356,#11640,#5827,.T.);
#14681=EDGE_CURVE('',#11357,#11639,#5828,.T.);
#14682=EDGE_CURVE('',#11358,#11638,#5829,.T.);
#14683=EDGE_CURVE('',#11518,#11821,#5830,.T.);
#14684=EDGE_CURVE('',#11361,#11635,#5831,.T.);
#14685=EDGE_CURVE('',#11415,#11823,#5832,.T.);
#14686=EDGE_CURVE('',#11416,#11822,#5833,.T.);
#14687=EDGE_CURVE('',#11365,#11633,#5834,.T.);
#14688=EDGE_CURVE('',#11366,#11632,#5835,.T.);
#14689=EDGE_CURVE('',#11367,#11631,#5836,.T.);
#14690=EDGE_CURVE('',#11368,#11630,#5837,.T.);
#14691=EDGE_CURVE('',#11369,#11629,#5838,.T.);
#14692=EDGE_CURVE('',#11370,#11628,#5839,.T.);
#14693=EDGE_CURVE('',#11371,#11627,#5840,.T.);
#14694=EDGE_CURVE('',#11372,#11626,#5841,.T.);
#14695=EDGE_CURVE('',#11373,#11625,#5842,.T.);
#14696=EDGE_CURVE('',#11374,#11624,#5843,.T.);
#14697=EDGE_CURVE('',#11375,#11623,#5844,.T.);
#14698=EDGE_CURVE('',#11376,#11622,#5845,.T.);
#14699=EDGE_CURVE('',#11377,#11621,#5846,.T.);
#14700=EDGE_CURVE('',#11378,#11620,#5847,.T.);
#14701=EDGE_CURVE('',#11511,#11824,#5848,.T.);
#14702=EDGE_CURVE('',#11381,#11617,#5849,.T.);
#14703=EDGE_CURVE('',#11407,#11826,#5850,.T.);
#14704=EDGE_CURVE('',#11408,#11825,#5851,.T.);
#14705=EDGE_CURVE('',#11385,#11615,#5852,.T.);
#14706=EDGE_CURVE('',#11386,#11614,#5853,.T.);
#14707=EDGE_CURVE('',#11387,#11613,#5854,.T.);
#14708=EDGE_CURVE('',#11388,#11612,#5855,.T.);
#14709=EDGE_CURVE('',#11389,#11611,#5856,.T.);
#14710=EDGE_CURVE('',#11390,#11610,#5857,.T.);
#14711=EDGE_CURVE('',#11391,#11609,#5858,.T.);
#14712=EDGE_CURVE('',#11392,#11608,#5859,.T.);
#14713=EDGE_CURVE('',#11393,#11607,#5860,.T.);
#14714=EDGE_CURVE('',#11394,#11606,#5861,.T.);
#14715=EDGE_CURVE('',#11395,#11605,#5862,.T.);
#14716=EDGE_CURVE('',#11396,#11604,#5863,.T.);
#14717=EDGE_CURVE('',#11397,#11603,#5864,.T.);
#14718=EDGE_CURVE('',#11398,#11602,#5865,.T.);
#14719=EDGE_CURVE('',#11504,#11827,#5866,.T.);
#14720=EDGE_CURVE('',#11163,#11599,#5867,.T.);
#14721=EDGE_CURVE('',#11160,#11829,#5868,.T.);
#14722=EDGE_CURVE('',#11161,#11828,#5869,.T.);
#14723=EDGE_CURVE('',#11165,#11597,#5870,.T.);
#14724=EDGE_CURVE('',#11166,#11596,#5871,.T.);
#14725=EDGE_CURVE('',#11167,#11595,#5872,.T.);
#14726=EDGE_CURVE('',#11168,#11594,#5873,.T.);
#14727=EDGE_CURVE('',#11169,#11593,#5874,.T.);
#14728=EDGE_CURVE('',#11170,#11592,#5875,.T.);
#14729=EDGE_CURVE('',#11171,#11591,#5876,.T.);
#14730=EDGE_CURVE('',#11172,#11590,#5877,.T.);
#14731=EDGE_CURVE('',#11173,#11589,#5878,.T.);
#14732=EDGE_CURVE('',#11174,#11588,#5879,.T.);
#14733=EDGE_CURVE('',#11175,#11587,#5880,.T.);
#14734=EDGE_CURVE('',#11176,#11586,#5881,.T.);
#14735=EDGE_CURVE('',#11177,#11585,#5882,.T.);
#14736=EDGE_CURVE('',#11178,#11584,#5883,.T.);
#14737=EDGE_CURVE('',#11497,#11830,#5884,.T.);
#14738=EDGE_CURVE('',#11401,#11839,#5885,.T.);
#14739=EDGE_CURVE('',#11839,#11839,#10572,.T.);
#14740=EDGE_CURVE('',#11840,#11840,#10573,.T.);
#14741=EDGE_CURVE('',#11841,#11841,#10574,.T.);
#14742=EDGE_CURVE('',#11841,#11840,#5886,.T.);
#14743=EDGE_CURVE('',#11842,#11842,#10575,.T.);
#14744=EDGE_CURVE('',#11842,#11841,#5887,.T.);
#14745=EDGE_CURVE('',#11843,#11843,#10576,.T.);
#14746=EDGE_CURVE('',#11843,#11796,#5888,.T.);
#14747=EDGE_CURVE('',#11844,#11845,#5889,.T.);
#14748=EDGE_CURVE('',#11845,#11846,#5890,.T.);
#14749=EDGE_CURVE('',#11846,#11847,#5891,.F.);
#14750=EDGE_CURVE('',#11847,#11848,#5892,.T.);
#14751=EDGE_CURVE('',#11848,#11849,#5893,.T.);
#14752=EDGE_CURVE('',#11849,#11844,#5894,.T.);
#14753=EDGE_CURVE('',#11850,#11846,#5895,.T.);
#14754=EDGE_CURVE('',#11845,#11851,#5896,.T.);
#14755=EDGE_CURVE('',#11851,#11852,#5897,.T.);
#14756=EDGE_CURVE('',#11852,#11853,#5898,.T.);
#14757=EDGE_CURVE('',#11853,#11854,#5899,.T.);
#14758=EDGE_CURVE('',#11854,#11855,#5900,.T.);
#14759=EDGE_CURVE('',#11855,#11856,#5901,.T.);
#14760=EDGE_CURVE('',#11856,#11857,#5902,.T.);
#14761=EDGE_CURVE('',#11857,#11858,#5903,.T.);
#14762=EDGE_CURVE('',#11858,#11859,#5904,.T.);
#14763=EDGE_CURVE('',#11859,#11860,#5905,.T.);
#14764=EDGE_CURVE('',#11860,#11861,#5906,.T.);
#14765=EDGE_CURVE('',#11861,#11862,#5907,.T.);
#14766=EDGE_CURVE('',#11862,#11863,#5908,.T.);
#14767=EDGE_CURVE('',#11863,#11864,#5909,.T.);
#14768=EDGE_CURVE('',#11864,#11865,#5910,.T.);
#14769=EDGE_CURVE('',#11865,#11866,#5911,.T.);
#14770=EDGE_CURVE('',#11867,#11866,#5912,.T.);
#14771=EDGE_CURVE('',#11867,#11868,#5913,.T.);
#14772=EDGE_CURVE('',#11868,#11869,#5914,.T.);
#14773=EDGE_CURVE('',#11870,#11869,#5915,.T.);
#14774=EDGE_CURVE('',#11870,#11871,#5916,.T.);
#14775=EDGE_CURVE('',#11871,#11872,#5917,.T.);
#14776=EDGE_CURVE('',#11872,#11873,#5918,.T.);
#14777=EDGE_CURVE('',#11873,#11874,#5919,.T.);
#14778=EDGE_CURVE('',#11874,#11875,#5920,.T.);
#14779=EDGE_CURVE('',#11875,#11876,#5921,.T.);
#14780=EDGE_CURVE('',#11876,#11877,#5922,.T.);
#14781=EDGE_CURVE('',#11877,#11878,#5923,.T.);
#14782=EDGE_CURVE('',#11878,#11879,#5924,.T.);
#14783=EDGE_CURVE('',#11879,#11880,#5925,.T.);
#14784=EDGE_CURVE('',#11880,#11881,#5926,.T.);
#14785=EDGE_CURVE('',#11881,#11882,#5927,.T.);
#14786=EDGE_CURVE('',#11882,#11883,#5928,.T.);
#14787=EDGE_CURVE('',#11883,#11884,#5929,.T.);
#14788=EDGE_CURVE('',#11884,#11885,#5930,.T.);
#14789=EDGE_CURVE('',#11885,#11886,#5931,.T.);
#14790=EDGE_CURVE('',#11887,#11886,#5932,.T.);
#14791=EDGE_CURVE('',#11887,#11888,#5933,.T.);
#14792=EDGE_CURVE('',#11888,#11889,#5934,.T.);
#14793=EDGE_CURVE('',#11890,#11889,#5935,.T.);
#14794=EDGE_CURVE('',#11890,#11891,#5936,.T.);
#14795=EDGE_CURVE('',#11891,#11892,#5937,.T.);
#14796=EDGE_CURVE('',#11892,#11893,#5938,.T.);
#14797=EDGE_CURVE('',#11893,#11894,#5939,.T.);
#14798=EDGE_CURVE('',#11894,#11895,#5940,.T.);
#14799=EDGE_CURVE('',#11895,#11896,#5941,.T.);
#14800=EDGE_CURVE('',#11896,#11897,#5942,.T.);
#14801=EDGE_CURVE('',#11897,#11898,#5943,.T.);
#14802=EDGE_CURVE('',#11898,#11899,#5944,.T.);
#14803=EDGE_CURVE('',#11899,#11900,#5945,.T.);
#14804=EDGE_CURVE('',#11900,#11901,#5946,.T.);
#14805=EDGE_CURVE('',#11901,#11902,#5947,.T.);
#14806=EDGE_CURVE('',#11902,#11903,#5948,.T.);
#14807=EDGE_CURVE('',#11903,#11904,#5949,.T.);
#14808=EDGE_CURVE('',#11904,#11905,#5950,.T.);
#14809=EDGE_CURVE('',#11905,#11906,#5951,.T.);
#14810=EDGE_CURVE('',#11907,#11906,#5952,.T.);
#14811=EDGE_CURVE('',#11907,#11908,#5953,.T.);
#14812=EDGE_CURVE('',#11908,#11909,#5954,.T.);
#14813=EDGE_CURVE('',#11910,#11909,#5955,.T.);
#14814=EDGE_CURVE('',#11910,#11911,#5956,.T.);
#14815=EDGE_CURVE('',#11911,#11912,#5957,.T.);
#14816=EDGE_CURVE('',#11912,#11913,#5958,.T.);
#14817=EDGE_CURVE('',#11913,#11914,#5959,.T.);
#14818=EDGE_CURVE('',#11914,#11915,#5960,.T.);
#14819=EDGE_CURVE('',#11915,#11916,#5961,.T.);
#14820=EDGE_CURVE('',#11916,#11917,#5962,.T.);
#14821=EDGE_CURVE('',#11917,#11918,#5963,.T.);
#14822=EDGE_CURVE('',#11918,#11919,#5964,.T.);
#14823=EDGE_CURVE('',#11919,#11920,#5965,.T.);
#14824=EDGE_CURVE('',#11920,#11921,#5966,.T.);
#14825=EDGE_CURVE('',#11921,#11922,#5967,.T.);
#14826=EDGE_CURVE('',#11922,#11923,#5968,.T.);
#14827=EDGE_CURVE('',#11923,#11924,#5969,.T.);
#14828=EDGE_CURVE('',#11924,#11925,#5970,.T.);
#14829=EDGE_CURVE('',#11925,#11926,#5971,.T.);
#14830=EDGE_CURVE('',#11927,#11926,#5972,.T.);
#14831=EDGE_CURVE('',#11927,#11928,#5973,.T.);
#14832=EDGE_CURVE('',#11928,#11929,#5974,.T.);
#14833=EDGE_CURVE('',#11930,#11929,#5975,.T.);
#14834=EDGE_CURVE('',#11930,#11931,#5976,.T.);
#14835=EDGE_CURVE('',#11931,#11932,#5977,.T.);
#14836=EDGE_CURVE('',#11932,#11933,#5978,.T.);
#14837=EDGE_CURVE('',#11933,#11934,#5979,.T.);
#14838=EDGE_CURVE('',#11934,#11935,#5980,.T.);
#14839=EDGE_CURVE('',#11935,#11936,#5981,.T.);
#14840=EDGE_CURVE('',#11936,#11937,#5982,.T.);
#14841=EDGE_CURVE('',#11937,#11938,#5983,.T.);
#14842=EDGE_CURVE('',#11938,#11939,#5984,.T.);
#14843=EDGE_CURVE('',#11939,#11940,#5985,.T.);
#14844=EDGE_CURVE('',#11940,#11941,#5986,.T.);
#14845=EDGE_CURVE('',#11941,#11942,#5987,.T.);
#14846=EDGE_CURVE('',#11942,#11943,#5988,.T.);
#14847=EDGE_CURVE('',#11943,#11944,#5989,.T.);
#14848=EDGE_CURVE('',#11944,#11945,#5990,.T.);
#14849=EDGE_CURVE('',#11945,#11946,#5991,.T.);
#14850=EDGE_CURVE('',#11947,#11946,#5992,.T.);
#14851=EDGE_CURVE('',#11947,#11948,#5993,.T.);
#14852=EDGE_CURVE('',#11948,#11949,#5994,.T.);
#14853=EDGE_CURVE('',#11950,#11949,#5995,.T.);
#14854=EDGE_CURVE('',#11950,#11951,#5996,.T.);
#14855=EDGE_CURVE('',#11951,#11952,#5997,.T.);
#14856=EDGE_CURVE('',#11952,#11953,#5998,.T.);
#14857=EDGE_CURVE('',#11953,#11954,#5999,.T.);
#14858=EDGE_CURVE('',#11954,#11955,#6000,.T.);
#14859=EDGE_CURVE('',#11955,#11956,#6001,.T.);
#14860=EDGE_CURVE('',#11956,#11957,#6002,.T.);
#14861=EDGE_CURVE('',#11957,#11958,#6003,.T.);
#14862=EDGE_CURVE('',#11958,#11959,#6004,.T.);
#14863=EDGE_CURVE('',#11959,#11960,#6005,.T.);
#14864=EDGE_CURVE('',#11960,#11961,#6006,.T.);
#14865=EDGE_CURVE('',#11961,#11962,#6007,.T.);
#14866=EDGE_CURVE('',#11962,#11963,#6008,.T.);
#14867=EDGE_CURVE('',#11963,#11964,#6009,.T.);
#14868=EDGE_CURVE('',#11964,#11965,#6010,.T.);
#14869=EDGE_CURVE('',#11965,#11966,#6011,.T.);
#14870=EDGE_CURVE('',#11967,#11966,#6012,.T.);
#14871=EDGE_CURVE('',#11967,#11968,#6013,.T.);
#14872=EDGE_CURVE('',#11968,#11969,#6014,.T.);
#14873=EDGE_CURVE('',#11970,#11969,#6015,.T.);
#14874=EDGE_CURVE('',#11970,#11971,#6016,.T.);
#14875=EDGE_CURVE('',#11971,#11972,#6017,.T.);
#14876=EDGE_CURVE('',#11972,#11973,#6018,.T.);
#14877=EDGE_CURVE('',#11973,#11974,#6019,.T.);
#14878=EDGE_CURVE('',#11974,#11975,#6020,.T.);
#14879=EDGE_CURVE('',#11975,#11976,#6021,.T.);
#14880=EDGE_CURVE('',#11976,#11977,#6022,.T.);
#14881=EDGE_CURVE('',#11977,#11978,#6023,.T.);
#14882=EDGE_CURVE('',#11978,#11979,#6024,.T.);
#14883=EDGE_CURVE('',#11979,#11980,#6025,.T.);
#14884=EDGE_CURVE('',#11980,#11981,#6026,.T.);
#14885=EDGE_CURVE('',#11981,#11982,#6027,.T.);
#14886=EDGE_CURVE('',#11982,#11983,#6028,.T.);
#14887=EDGE_CURVE('',#11983,#11984,#6029,.T.);
#14888=EDGE_CURVE('',#11984,#11985,#6030,.T.);
#14889=EDGE_CURVE('',#11985,#11986,#6031,.T.);
#14890=EDGE_CURVE('',#11987,#11986,#6032,.T.);
#14891=EDGE_CURVE('',#11987,#11988,#6033,.T.);
#14892=EDGE_CURVE('',#11988,#11989,#6034,.T.);
#14893=EDGE_CURVE('',#11990,#11989,#6035,.T.);
#14894=EDGE_CURVE('',#11990,#11991,#6036,.T.);
#14895=EDGE_CURVE('',#11991,#11992,#6037,.T.);
#14896=EDGE_CURVE('',#11992,#11993,#6038,.T.);
#14897=EDGE_CURVE('',#11993,#11994,#6039,.T.);
#14898=EDGE_CURVE('',#11994,#11995,#6040,.T.);
#14899=EDGE_CURVE('',#11995,#11996,#6041,.T.);
#14900=EDGE_CURVE('',#11996,#11997,#6042,.T.);
#14901=EDGE_CURVE('',#11997,#11998,#6043,.T.);
#14902=EDGE_CURVE('',#11998,#11999,#6044,.T.);
#14903=EDGE_CURVE('',#11999,#12000,#6045,.T.);
#14904=EDGE_CURVE('',#12000,#12001,#6046,.T.);
#14905=EDGE_CURVE('',#12001,#12002,#6047,.T.);
#14906=EDGE_CURVE('',#12002,#12003,#6048,.T.);
#14907=EDGE_CURVE('',#12003,#12004,#6049,.T.);
#14908=EDGE_CURVE('',#12004,#12005,#6050,.T.);
#14909=EDGE_CURVE('',#12005,#12006,#6051,.T.);
#14910=EDGE_CURVE('',#12007,#12006,#6052,.T.);
#14911=EDGE_CURVE('',#12007,#12008,#6053,.T.);
#14912=EDGE_CURVE('',#12008,#12009,#6054,.T.);
#14913=EDGE_CURVE('',#12010,#12009,#6055,.T.);
#14914=EDGE_CURVE('',#12010,#12011,#6056,.T.);
#14915=EDGE_CURVE('',#12011,#12012,#6057,.T.);
#14916=EDGE_CURVE('',#12012,#12013,#6058,.T.);
#14917=EDGE_CURVE('',#12013,#12014,#6059,.T.);
#14918=EDGE_CURVE('',#12014,#12015,#6060,.T.);
#14919=EDGE_CURVE('',#12015,#12016,#6061,.T.);
#14920=EDGE_CURVE('',#12016,#12017,#6062,.T.);
#14921=EDGE_CURVE('',#12017,#12018,#6063,.T.);
#14922=EDGE_CURVE('',#12018,#12019,#6064,.T.);
#14923=EDGE_CURVE('',#12019,#12020,#6065,.T.);
#14924=EDGE_CURVE('',#12020,#12021,#6066,.T.);
#14925=EDGE_CURVE('',#12021,#12022,#6067,.T.);
#14926=EDGE_CURVE('',#12022,#12023,#6068,.T.);
#14927=EDGE_CURVE('',#12023,#12024,#6069,.T.);
#14928=EDGE_CURVE('',#12024,#12025,#6070,.T.);
#14929=EDGE_CURVE('',#12025,#12026,#6071,.T.);
#14930=EDGE_CURVE('',#12027,#12026,#6072,.T.);
#14931=EDGE_CURVE('',#12027,#12028,#6073,.T.);
#14932=EDGE_CURVE('',#12028,#12029,#6074,.T.);
#14933=EDGE_CURVE('',#12030,#12029,#6075,.T.);
#14934=EDGE_CURVE('',#12030,#12031,#6076,.T.);
#14935=EDGE_CURVE('',#12031,#12032,#6077,.T.);
#14936=EDGE_CURVE('',#12032,#12033,#6078,.T.);
#14937=EDGE_CURVE('',#12033,#12034,#6079,.T.);
#14938=EDGE_CURVE('',#12034,#12035,#6080,.T.);
#14939=EDGE_CURVE('',#12035,#12036,#6081,.T.);
#14940=EDGE_CURVE('',#12036,#12037,#6082,.T.);
#14941=EDGE_CURVE('',#12037,#12038,#6083,.T.);
#14942=EDGE_CURVE('',#12038,#12039,#6084,.T.);
#14943=EDGE_CURVE('',#12039,#12040,#6085,.T.);
#14944=EDGE_CURVE('',#12040,#12041,#6086,.T.);
#14945=EDGE_CURVE('',#12041,#12042,#6087,.T.);
#14946=EDGE_CURVE('',#12042,#12043,#6088,.T.);
#14947=EDGE_CURVE('',#12043,#12044,#6089,.T.);
#14948=EDGE_CURVE('',#12044,#12045,#6090,.T.);
#14949=EDGE_CURVE('',#12045,#12046,#6091,.T.);
#14950=EDGE_CURVE('',#12047,#12046,#6092,.T.);
#14951=EDGE_CURVE('',#12047,#12048,#6093,.T.);
#14952=EDGE_CURVE('',#12048,#12049,#6094,.T.);
#14953=EDGE_CURVE('',#12050,#12049,#6095,.T.);
#14954=EDGE_CURVE('',#12050,#12051,#6096,.T.);
#14955=EDGE_CURVE('',#12051,#12052,#6097,.T.);
#14956=EDGE_CURVE('',#12052,#12053,#6098,.T.);
#14957=EDGE_CURVE('',#12053,#12054,#6099,.T.);
#14958=EDGE_CURVE('',#12054,#12055,#6100,.T.);
#14959=EDGE_CURVE('',#12055,#12056,#6101,.T.);
#14960=EDGE_CURVE('',#12056,#12057,#6102,.T.);
#14961=EDGE_CURVE('',#12057,#12058,#6103,.T.);
#14962=EDGE_CURVE('',#12058,#12059,#6104,.T.);
#14963=EDGE_CURVE('',#12059,#12060,#6105,.T.);
#14964=EDGE_CURVE('',#12060,#12061,#6106,.T.);
#14965=EDGE_CURVE('',#12061,#12062,#6107,.T.);
#14966=EDGE_CURVE('',#12062,#12063,#6108,.T.);
#14967=EDGE_CURVE('',#12063,#12064,#6109,.T.);
#14968=EDGE_CURVE('',#12064,#12065,#6110,.T.);
#14969=EDGE_CURVE('',#12065,#12066,#6111,.T.);
#14970=EDGE_CURVE('',#12067,#12066,#6112,.T.);
#14971=EDGE_CURVE('',#12067,#12068,#6113,.T.);
#14972=EDGE_CURVE('',#12068,#12069,#6114,.T.);
#14973=EDGE_CURVE('',#12070,#12069,#6115,.T.);
#14974=EDGE_CURVE('',#12070,#12071,#6116,.T.);
#14975=EDGE_CURVE('',#12071,#12072,#6117,.T.);
#14976=EDGE_CURVE('',#12072,#12073,#6118,.T.);
#14977=EDGE_CURVE('',#12073,#12074,#6119,.T.);
#14978=EDGE_CURVE('',#12074,#12075,#6120,.T.);
#14979=EDGE_CURVE('',#12075,#12076,#6121,.T.);
#14980=EDGE_CURVE('',#12076,#12077,#6122,.T.);
#14981=EDGE_CURVE('',#12077,#12078,#6123,.T.);
#14982=EDGE_CURVE('',#12078,#12079,#6124,.T.);
#14983=EDGE_CURVE('',#12079,#12080,#6125,.T.);
#14984=EDGE_CURVE('',#12080,#12081,#6126,.T.);
#14985=EDGE_CURVE('',#12081,#12082,#6127,.T.);
#14986=EDGE_CURVE('',#12082,#12083,#6128,.T.);
#14987=EDGE_CURVE('',#12083,#12084,#6129,.T.);
#14988=EDGE_CURVE('',#12084,#12085,#6130,.T.);
#14989=EDGE_CURVE('',#12085,#12086,#6131,.T.);
#14990=EDGE_CURVE('',#12087,#12086,#6132,.T.);
#14991=EDGE_CURVE('',#12087,#11850,#6133,.T.);
#14992=EDGE_CURVE('',#12088,#12088,#10577,.T.);
#14993=EDGE_CURVE('',#11844,#12089,#6134,.T.);
#14994=EDGE_CURVE('',#12090,#12089,#6135,.T.);
#14995=EDGE_CURVE('',#12091,#12090,#6136,.T.);
#14996=EDGE_CURVE('',#11851,#12091,#6137,.T.);
#14997=EDGE_CURVE('',#11849,#12092,#6138,.T.);
#14998=EDGE_CURVE('',#12089,#12092,#6139,.T.);
#14999=EDGE_CURVE('',#12093,#12070,#6140,.T.);
#15000=EDGE_CURVE('',#12069,#12094,#6141,.F.);
#15001=EDGE_CURVE('',#12094,#12095,#6142,.T.);
#15002=EDGE_CURVE('',#12095,#12096,#6143,.T.);
#15003=EDGE_CURVE('',#12096,#12093,#6144,.T.);
#15004=EDGE_CURVE('',#12093,#12097,#6145,.T.);
#15005=EDGE_CURVE('',#12098,#12097,#6146,.T.);
#15006=EDGE_CURVE('',#12099,#12098,#6147,.T.);
#15007=EDGE_CURVE('',#12071,#12099,#6148,.T.);
#15008=EDGE_CURVE('',#12096,#12100,#6149,.T.);
#15009=EDGE_CURVE('',#12097,#12100,#6150,.T.);
#15010=EDGE_CURVE('',#12101,#12050,#6151,.T.);
#15011=EDGE_CURVE('',#12049,#12102,#6152,.F.);
#15012=EDGE_CURVE('',#12102,#12103,#6153,.T.);
#15013=EDGE_CURVE('',#12103,#12104,#6154,.T.);
#15014=EDGE_CURVE('',#12104,#12101,#6155,.T.);
#15015=EDGE_CURVE('',#12101,#12105,#6156,.T.);
#15016=EDGE_CURVE('',#12106,#12105,#6157,.T.);
#15017=EDGE_CURVE('',#12107,#12106,#6158,.T.);
#15018=EDGE_CURVE('',#12051,#12107,#6159,.T.);
#15019=EDGE_CURVE('',#12104,#12108,#6160,.T.);
#15020=EDGE_CURVE('',#12105,#12108,#6161,.T.);
#15021=EDGE_CURVE('',#12109,#12030,#6162,.T.);
#15022=EDGE_CURVE('',#12029,#12110,#6163,.F.);
#15023=EDGE_CURVE('',#12110,#12111,#6164,.T.);
#15024=EDGE_CURVE('',#12111,#12112,#6165,.T.);
#15025=EDGE_CURVE('',#12112,#12109,#6166,.T.);
#15026=EDGE_CURVE('',#12109,#12113,#6167,.T.);
#15027=EDGE_CURVE('',#12114,#12113,#6168,.T.);
#15028=EDGE_CURVE('',#12115,#12114,#6169,.T.);
#15029=EDGE_CURVE('',#12031,#12115,#6170,.T.);
#15030=EDGE_CURVE('',#12112,#12116,#6171,.T.);
#15031=EDGE_CURVE('',#12113,#12116,#6172,.T.);
#15032=EDGE_CURVE('',#12117,#12010,#6173,.T.);
#15033=EDGE_CURVE('',#12009,#12118,#6174,.F.);
#15034=EDGE_CURVE('',#12118,#12119,#6175,.T.);
#15035=EDGE_CURVE('',#12119,#12120,#6176,.T.);
#15036=EDGE_CURVE('',#12120,#12117,#6177,.T.);
#15037=EDGE_CURVE('',#12117,#12121,#6178,.T.);
#15038=EDGE_CURVE('',#12122,#12121,#6179,.T.);
#15039=EDGE_CURVE('',#12123,#12122,#6180,.T.);
#15040=EDGE_CURVE('',#12011,#12123,#6181,.T.);
#15041=EDGE_CURVE('',#12120,#12124,#6182,.T.);
#15042=EDGE_CURVE('',#12121,#12124,#6183,.T.);
#15043=EDGE_CURVE('',#12125,#11990,#6184,.T.);
#15044=EDGE_CURVE('',#11989,#12126,#6185,.F.);
#15045=EDGE_CURVE('',#12126,#12127,#6186,.T.);
#15046=EDGE_CURVE('',#12127,#12128,#6187,.T.);
#15047=EDGE_CURVE('',#12128,#12125,#6188,.T.);
#15048=EDGE_CURVE('',#12125,#12129,#6189,.T.);
#15049=EDGE_CURVE('',#12130,#12129,#6190,.T.);
#15050=EDGE_CURVE('',#12131,#12130,#6191,.T.);
#15051=EDGE_CURVE('',#11991,#12131,#6192,.T.);
#15052=EDGE_CURVE('',#12128,#12132,#6193,.T.);
#15053=EDGE_CURVE('',#12129,#12132,#6194,.T.);
#15054=EDGE_CURVE('',#12133,#11970,#6195,.T.);
#15055=EDGE_CURVE('',#11969,#12134,#6196,.F.);
#15056=EDGE_CURVE('',#12134,#12135,#6197,.T.);
#15057=EDGE_CURVE('',#12135,#12136,#6198,.T.);
#15058=EDGE_CURVE('',#12136,#12133,#6199,.T.);
#15059=EDGE_CURVE('',#12133,#12137,#6200,.T.);
#15060=EDGE_CURVE('',#12138,#12137,#6201,.T.);
#15061=EDGE_CURVE('',#12139,#12138,#6202,.T.);
#15062=EDGE_CURVE('',#11971,#12139,#6203,.T.);
#15063=EDGE_CURVE('',#12136,#12140,#6204,.T.);
#15064=EDGE_CURVE('',#12137,#12140,#6205,.T.);
#15065=EDGE_CURVE('',#12141,#11950,#6206,.T.);
#15066=EDGE_CURVE('',#11949,#12142,#6207,.F.);
#15067=EDGE_CURVE('',#12142,#12143,#6208,.T.);
#15068=EDGE_CURVE('',#12143,#12144,#6209,.T.);
#15069=EDGE_CURVE('',#12144,#12141,#6210,.T.);
#15070=EDGE_CURVE('',#12141,#12145,#6211,.T.);
#15071=EDGE_CURVE('',#12146,#12145,#6212,.T.);
#15072=EDGE_CURVE('',#12147,#12146,#6213,.T.);
#15073=EDGE_CURVE('',#11951,#12147,#6214,.T.);
#15074=EDGE_CURVE('',#12144,#12148,#6215,.T.);
#15075=EDGE_CURVE('',#12145,#12148,#6216,.T.);
#15076=EDGE_CURVE('',#12149,#11930,#6217,.T.);
#15077=EDGE_CURVE('',#11929,#12150,#6218,.F.);
#15078=EDGE_CURVE('',#12150,#12151,#6219,.T.);
#15079=EDGE_CURVE('',#12151,#12152,#6220,.T.);
#15080=EDGE_CURVE('',#12152,#12149,#6221,.T.);
#15081=EDGE_CURVE('',#12149,#12153,#6222,.T.);
#15082=EDGE_CURVE('',#12154,#12153,#6223,.T.);
#15083=EDGE_CURVE('',#12155,#12154,#6224,.T.);
#15084=EDGE_CURVE('',#11931,#12155,#6225,.T.);
#15085=EDGE_CURVE('',#12152,#12156,#6226,.T.);
#15086=EDGE_CURVE('',#12153,#12156,#6227,.T.);
#15087=EDGE_CURVE('',#12157,#11910,#6228,.T.);
#15088=EDGE_CURVE('',#11909,#12158,#6229,.F.);
#15089=EDGE_CURVE('',#12158,#12159,#6230,.T.);
#15090=EDGE_CURVE('',#12159,#12160,#6231,.T.);
#15091=EDGE_CURVE('',#12160,#12157,#6232,.T.);
#15092=EDGE_CURVE('',#12157,#12161,#6233,.T.);
#15093=EDGE_CURVE('',#12162,#12161,#6234,.T.);
#15094=EDGE_CURVE('',#12163,#12162,#6235,.T.);
#15095=EDGE_CURVE('',#11911,#12163,#6236,.T.);
#15096=EDGE_CURVE('',#12160,#12164,#6237,.T.);
#15097=EDGE_CURVE('',#12161,#12164,#6238,.T.);
#15098=EDGE_CURVE('',#12165,#11890,#6239,.T.);
#15099=EDGE_CURVE('',#11889,#12166,#6240,.F.);
#15100=EDGE_CURVE('',#12166,#12167,#6241,.T.);
#15101=EDGE_CURVE('',#12167,#12168,#6242,.T.);
#15102=EDGE_CURVE('',#12168,#12165,#6243,.T.);
#15103=EDGE_CURVE('',#12165,#12169,#6244,.T.);
#15104=EDGE_CURVE('',#12170,#12169,#6245,.T.);
#15105=EDGE_CURVE('',#12171,#12170,#6246,.T.);
#15106=EDGE_CURVE('',#11891,#12171,#6247,.T.);
#15107=EDGE_CURVE('',#12168,#12172,#6248,.T.);
#15108=EDGE_CURVE('',#12169,#12172,#6249,.T.);
#15109=EDGE_CURVE('',#12173,#11870,#6250,.T.);
#15110=EDGE_CURVE('',#11869,#12174,#6251,.F.);
#15111=EDGE_CURVE('',#12174,#12175,#6252,.T.);
#15112=EDGE_CURVE('',#12175,#12176,#6253,.T.);
#15113=EDGE_CURVE('',#12176,#12173,#6254,.T.);
#15114=EDGE_CURVE('',#12173,#12177,#6255,.T.);
#15115=EDGE_CURVE('',#12178,#12177,#6256,.T.);
#15116=EDGE_CURVE('',#12179,#12178,#6257,.T.);
#15117=EDGE_CURVE('',#11871,#12179,#6258,.T.);
#15118=EDGE_CURVE('',#12176,#12180,#6259,.T.);
#15119=EDGE_CURVE('',#12177,#12180,#6260,.T.);
#15120=EDGE_CURVE('',#12181,#12182,#6261,.T.);
#15121=EDGE_CURVE('',#12182,#12183,#6262,.T.);
#15122=EDGE_CURVE('',#12183,#11867,#6263,.F.);
#15123=EDGE_CURVE('',#11866,#12184,#6264,.T.);
#15124=EDGE_CURVE('',#12184,#12181,#6265,.T.);
#15125=EDGE_CURVE('',#12182,#12185,#6266,.T.);
#15126=EDGE_CURVE('',#12186,#12185,#6267,.T.);
#15127=EDGE_CURVE('',#12183,#12186,#6268,.T.);
#15128=EDGE_CURVE('',#12181,#12187,#6269,.T.);
#15129=EDGE_CURVE('',#12185,#12187,#6270,.T.);
#15130=EDGE_CURVE('',#12188,#12189,#6271,.T.);
#15131=EDGE_CURVE('',#12189,#12190,#6272,.T.);
#15132=EDGE_CURVE('',#12190,#12087,#6273,.F.);
#15133=EDGE_CURVE('',#12086,#12191,#6274,.T.);
#15134=EDGE_CURVE('',#12191,#12188,#6275,.T.);
#15135=EDGE_CURVE('',#12189,#12192,#6276,.T.);
#15136=EDGE_CURVE('',#12193,#12192,#6277,.T.);
#15137=EDGE_CURVE('',#12190,#12193,#6278,.T.);
#15138=EDGE_CURVE('',#12188,#12194,#6279,.T.);
#15139=EDGE_CURVE('',#12192,#12194,#6280,.T.);
#15140=EDGE_CURVE('',#12195,#12196,#6281,.T.);
#15141=EDGE_CURVE('',#12196,#12197,#6282,.T.);
#15142=EDGE_CURVE('',#12197,#12067,#6283,.F.);
#15143=EDGE_CURVE('',#12066,#12198,#6284,.T.);
#15144=EDGE_CURVE('',#12198,#12195,#6285,.T.);
#15145=EDGE_CURVE('',#12196,#12199,#6286,.T.);
#15146=EDGE_CURVE('',#12200,#12199,#6287,.T.);
#15147=EDGE_CURVE('',#12197,#12200,#6288,.T.);
#15148=EDGE_CURVE('',#12195,#12201,#6289,.T.);
#15149=EDGE_CURVE('',#12199,#12201,#6290,.T.);
#15150=EDGE_CURVE('',#12202,#12203,#6291,.T.);
#15151=EDGE_CURVE('',#12203,#12204,#6292,.T.);
#15152=EDGE_CURVE('',#12204,#12047,#6293,.F.);
#15153=EDGE_CURVE('',#12046,#12205,#6294,.T.);
#15154=EDGE_CURVE('',#12205,#12202,#6295,.T.);
#15155=EDGE_CURVE('',#12203,#12206,#6296,.T.);
#15156=EDGE_CURVE('',#12207,#12206,#6297,.T.);
#15157=EDGE_CURVE('',#12204,#12207,#6298,.T.);
#15158=EDGE_CURVE('',#12202,#12208,#6299,.T.);
#15159=EDGE_CURVE('',#12206,#12208,#6300,.T.);
#15160=EDGE_CURVE('',#12209,#12210,#6301,.T.);
#15161=EDGE_CURVE('',#12210,#12211,#6302,.T.);
#15162=EDGE_CURVE('',#12211,#12027,#6303,.F.);
#15163=EDGE_CURVE('',#12026,#12212,#6304,.T.);
#15164=EDGE_CURVE('',#12212,#12209,#6305,.T.);
#15165=EDGE_CURVE('',#12210,#12213,#6306,.T.);
#15166=EDGE_CURVE('',#12214,#12213,#6307,.T.);
#15167=EDGE_CURVE('',#12211,#12214,#6308,.T.);
#15168=EDGE_CURVE('',#12209,#12215,#6309,.T.);
#15169=EDGE_CURVE('',#12213,#12215,#6310,.T.);
#15170=EDGE_CURVE('',#12216,#12217,#6311,.T.);
#15171=EDGE_CURVE('',#12217,#12218,#6312,.T.);
#15172=EDGE_CURVE('',#12218,#12007,#6313,.F.);
#15173=EDGE_CURVE('',#12006,#12219,#6314,.T.);
#15174=EDGE_CURVE('',#12219,#12216,#6315,.T.);
#15175=EDGE_CURVE('',#12217,#12220,#6316,.T.);
#15176=EDGE_CURVE('',#12221,#12220,#6317,.T.);
#15177=EDGE_CURVE('',#12218,#12221,#6318,.T.);
#15178=EDGE_CURVE('',#12216,#12222,#6319,.T.);
#15179=EDGE_CURVE('',#12220,#12222,#6320,.T.);
#15180=EDGE_CURVE('',#12223,#12224,#6321,.T.);
#15181=EDGE_CURVE('',#12224,#12225,#6322,.T.);
#15182=EDGE_CURVE('',#12225,#11987,#6323,.F.);
#15183=EDGE_CURVE('',#11986,#12226,#6324,.T.);
#15184=EDGE_CURVE('',#12226,#12223,#6325,.T.);
#15185=EDGE_CURVE('',#12224,#12227,#6326,.T.);
#15186=EDGE_CURVE('',#12228,#12227,#6327,.T.);
#15187=EDGE_CURVE('',#12225,#12228,#6328,.T.);
#15188=EDGE_CURVE('',#12223,#12229,#6329,.T.);
#15189=EDGE_CURVE('',#12227,#12229,#6330,.T.);
#15190=EDGE_CURVE('',#12230,#12231,#6331,.T.);
#15191=EDGE_CURVE('',#12231,#12232,#6332,.T.);
#15192=EDGE_CURVE('',#12232,#11967,#6333,.F.);
#15193=EDGE_CURVE('',#11966,#12233,#6334,.T.);
#15194=EDGE_CURVE('',#12233,#12230,#6335,.T.);
#15195=EDGE_CURVE('',#12231,#12234,#6336,.T.);
#15196=EDGE_CURVE('',#12235,#12234,#6337,.T.);
#15197=EDGE_CURVE('',#12232,#12235,#6338,.T.);
#15198=EDGE_CURVE('',#12230,#12236,#6339,.T.);
#15199=EDGE_CURVE('',#12234,#12236,#6340,.T.);
#15200=EDGE_CURVE('',#12237,#12238,#6341,.T.);
#15201=EDGE_CURVE('',#12238,#12239,#6342,.T.);
#15202=EDGE_CURVE('',#12239,#11947,#6343,.F.);
#15203=EDGE_CURVE('',#11946,#12240,#6344,.T.);
#15204=EDGE_CURVE('',#12240,#12237,#6345,.T.);
#15205=EDGE_CURVE('',#12238,#12241,#6346,.T.);
#15206=EDGE_CURVE('',#12242,#12241,#6347,.T.);
#15207=EDGE_CURVE('',#12239,#12242,#6348,.T.);
#15208=EDGE_CURVE('',#12237,#12243,#6349,.T.);
#15209=EDGE_CURVE('',#12241,#12243,#6350,.T.);
#15210=EDGE_CURVE('',#12244,#12245,#6351,.T.);
#15211=EDGE_CURVE('',#12245,#12246,#6352,.T.);
#15212=EDGE_CURVE('',#12246,#11927,#6353,.F.);
#15213=EDGE_CURVE('',#11926,#12247,#6354,.T.);
#15214=EDGE_CURVE('',#12247,#12244,#6355,.T.);
#15215=EDGE_CURVE('',#12245,#12248,#6356,.T.);
#15216=EDGE_CURVE('',#12249,#12248,#6357,.T.);
#15217=EDGE_CURVE('',#12246,#12249,#6358,.T.);
#15218=EDGE_CURVE('',#12244,#12250,#6359,.T.);
#15219=EDGE_CURVE('',#12248,#12250,#6360,.T.);
#15220=EDGE_CURVE('',#12251,#12252,#6361,.T.);
#15221=EDGE_CURVE('',#12252,#12253,#6362,.T.);
#15222=EDGE_CURVE('',#12253,#11907,#6363,.F.);
#15223=EDGE_CURVE('',#11906,#12254,#6364,.T.);
#15224=EDGE_CURVE('',#12254,#12251,#6365,.T.);
#15225=EDGE_CURVE('',#12252,#12255,#6366,.T.);
#15226=EDGE_CURVE('',#12256,#12255,#6367,.T.);
#15227=EDGE_CURVE('',#12253,#12256,#6368,.T.);
#15228=EDGE_CURVE('',#12251,#12257,#6369,.T.);
#15229=EDGE_CURVE('',#12255,#12257,#6370,.T.);
#15230=EDGE_CURVE('',#12258,#12259,#6371,.T.);
#15231=EDGE_CURVE('',#12259,#12260,#6372,.T.);
#15232=EDGE_CURVE('',#12260,#11887,#6373,.F.);
#15233=EDGE_CURVE('',#11886,#12261,#6374,.T.);
#15234=EDGE_CURVE('',#12261,#12258,#6375,.T.);
#15235=EDGE_CURVE('',#12259,#12262,#6376,.T.);
#15236=EDGE_CURVE('',#12263,#12262,#6377,.T.);
#15237=EDGE_CURVE('',#12260,#12263,#6378,.T.);
#15238=EDGE_CURVE('',#12258,#12264,#6379,.T.);
#15239=EDGE_CURVE('',#12262,#12264,#6380,.T.);
#15240=EDGE_CURVE('',#12180,#12265,#6381,.T.);
#15241=EDGE_CURVE('',#12265,#12266,#6382,.T.);
#15242=EDGE_CURVE('',#12266,#12267,#6383,.F.);
#15243=EDGE_CURVE('',#12267,#12178,#6384,.T.);
#15244=EDGE_CURVE('',#12267,#12268,#6385,.T.);
#15245=EDGE_CURVE('',#12268,#12269,#6386,.T.);
#15246=EDGE_CURVE('',#12270,#12269,#6387,.T.);
#15247=EDGE_CURVE('',#12270,#12271,#6388,.T.);
#15248=EDGE_CURVE('',#12271,#12272,#6389,.T.);
#15249=EDGE_CURVE('',#12272,#12273,#6390,.T.);
#15250=EDGE_CURVE('',#12273,#12274,#6391,.T.);
#15251=EDGE_CURVE('',#12274,#12275,#6392,.T.);
#15252=EDGE_CURVE('',#12275,#12276,#6393,.T.);
#15253=EDGE_CURVE('',#12276,#12277,#6394,.T.);
#15254=EDGE_CURVE('',#12277,#12278,#6395,.T.);
#15255=EDGE_CURVE('',#12278,#12279,#6396,.T.);
#15256=EDGE_CURVE('',#12279,#12280,#6397,.T.);
#15257=EDGE_CURVE('',#12280,#12281,#6398,.T.);
#15258=EDGE_CURVE('',#12281,#12282,#6399,.T.);
#15259=EDGE_CURVE('',#12282,#12283,#6400,.T.);
#15260=EDGE_CURVE('',#12283,#12284,#6401,.T.);
#15261=EDGE_CURVE('',#12284,#12091,#6402,.T.);
#15262=EDGE_CURVE('',#12285,#12090,#6403,.T.);
#15263=EDGE_CURVE('',#12285,#12286,#6404,.T.);
#15264=EDGE_CURVE('',#12286,#12287,#6405,.T.);
#15265=EDGE_CURVE('',#12288,#12287,#6406,.T.);
#15266=EDGE_CURVE('',#12288,#12289,#6407,.T.);
#15267=EDGE_CURVE('',#12289,#12290,#6408,.T.);
#15268=EDGE_CURVE('',#12290,#12291,#6409,.T.);
#15269=EDGE_CURVE('',#12291,#12292,#6410,.T.);
#15270=EDGE_CURVE('',#12292,#12293,#6411,.T.);
#15271=EDGE_CURVE('',#12293,#12294,#6412,.T.);
#15272=EDGE_CURVE('',#12294,#12295,#6413,.T.);
#15273=EDGE_CURVE('',#12295,#12296,#6414,.T.);
#15274=EDGE_CURVE('',#12296,#12297,#6415,.T.);
#15275=EDGE_CURVE('',#12297,#12298,#6416,.T.);
#15276=EDGE_CURVE('',#12298,#12299,#6417,.T.);
#15277=EDGE_CURVE('',#12299,#12300,#6418,.T.);
#15278=EDGE_CURVE('',#12300,#12301,#6419,.T.);
#15279=EDGE_CURVE('',#12301,#12302,#6420,.T.);
#15280=EDGE_CURVE('',#12302,#12099,#6421,.T.);
#15281=EDGE_CURVE('',#12303,#12098,#6422,.T.);
#15282=EDGE_CURVE('',#12303,#12304,#6423,.T.);
#15283=EDGE_CURVE('',#12304,#12305,#6424,.T.);
#15284=EDGE_CURVE('',#12306,#12305,#6425,.T.);
#15285=EDGE_CURVE('',#12306,#12307,#6426,.T.);
#15286=EDGE_CURVE('',#12307,#12308,#6427,.T.);
#15287=EDGE_CURVE('',#12308,#12309,#6428,.T.);
#15288=EDGE_CURVE('',#12309,#12310,#6429,.T.);
#15289=EDGE_CURVE('',#12310,#12311,#6430,.T.);
#15290=EDGE_CURVE('',#12311,#12312,#6431,.T.);
#15291=EDGE_CURVE('',#12312,#12313,#6432,.T.);
#15292=EDGE_CURVE('',#12313,#12314,#6433,.T.);
#15293=EDGE_CURVE('',#12314,#12315,#6434,.T.);
#15294=EDGE_CURVE('',#12315,#12316,#6435,.T.);
#15295=EDGE_CURVE('',#12316,#12317,#6436,.T.);
#15296=EDGE_CURVE('',#12317,#12318,#6437,.T.);
#15297=EDGE_CURVE('',#12318,#12319,#6438,.T.);
#15298=EDGE_CURVE('',#12319,#12320,#6439,.T.);
#15299=EDGE_CURVE('',#12320,#12107,#6440,.T.);
#15300=EDGE_CURVE('',#12321,#12106,#6441,.T.);
#15301=EDGE_CURVE('',#12321,#12322,#6442,.T.);
#15302=EDGE_CURVE('',#12322,#12323,#6443,.T.);
#15303=EDGE_CURVE('',#12324,#12323,#6444,.T.);
#15304=EDGE_CURVE('',#12324,#12325,#6445,.T.);
#15305=EDGE_CURVE('',#12325,#12326,#6446,.T.);
#15306=EDGE_CURVE('',#12326,#12327,#6447,.T.);
#15307=EDGE_CURVE('',#12327,#12328,#6448,.T.);
#15308=EDGE_CURVE('',#12328,#12329,#6449,.T.);
#15309=EDGE_CURVE('',#12329,#12330,#6450,.T.);
#15310=EDGE_CURVE('',#12330,#12331,#6451,.T.);
#15311=EDGE_CURVE('',#12331,#12332,#6452,.T.);
#15312=EDGE_CURVE('',#12332,#12333,#6453,.T.);
#15313=EDGE_CURVE('',#12333,#12334,#6454,.T.);
#15314=EDGE_CURVE('',#12334,#12335,#6455,.T.);
#15315=EDGE_CURVE('',#12335,#12336,#6456,.T.);
#15316=EDGE_CURVE('',#12336,#12337,#6457,.T.);
#15317=EDGE_CURVE('',#12337,#12338,#6458,.T.);
#15318=EDGE_CURVE('',#12338,#12115,#6459,.T.);
#15319=EDGE_CURVE('',#12339,#12114,#6460,.T.);
#15320=EDGE_CURVE('',#12339,#12340,#6461,.T.);
#15321=EDGE_CURVE('',#12340,#12341,#6462,.T.);
#15322=EDGE_CURVE('',#12342,#12341,#6463,.T.);
#15323=EDGE_CURVE('',#12342,#12343,#6464,.T.);
#15324=EDGE_CURVE('',#12343,#12344,#6465,.T.);
#15325=EDGE_CURVE('',#12344,#12345,#6466,.T.);
#15326=EDGE_CURVE('',#12345,#12346,#6467,.T.);
#15327=EDGE_CURVE('',#12346,#12347,#6468,.T.);
#15328=EDGE_CURVE('',#12347,#12348,#6469,.T.);
#15329=EDGE_CURVE('',#12348,#12349,#6470,.T.);
#15330=EDGE_CURVE('',#12349,#12350,#6471,.T.);
#15331=EDGE_CURVE('',#12350,#12351,#6472,.T.);
#15332=EDGE_CURVE('',#12351,#12352,#6473,.T.);
#15333=EDGE_CURVE('',#12352,#12353,#6474,.T.);
#15334=EDGE_CURVE('',#12353,#12354,#6475,.T.);
#15335=EDGE_CURVE('',#12354,#12355,#6476,.T.);
#15336=EDGE_CURVE('',#12355,#12356,#6477,.T.);
#15337=EDGE_CURVE('',#12356,#12123,#6478,.T.);
#15338=EDGE_CURVE('',#12357,#12122,#6479,.T.);
#15339=EDGE_CURVE('',#12357,#12358,#6480,.T.);
#15340=EDGE_CURVE('',#12358,#12359,#6481,.T.);
#15341=EDGE_CURVE('',#12360,#12359,#6482,.T.);
#15342=EDGE_CURVE('',#12360,#12361,#6483,.T.);
#15343=EDGE_CURVE('',#12361,#12362,#6484,.T.);
#15344=EDGE_CURVE('',#12362,#12363,#6485,.T.);
#15345=EDGE_CURVE('',#12363,#12364,#6486,.T.);
#15346=EDGE_CURVE('',#12364,#12365,#6487,.T.);
#15347=EDGE_CURVE('',#12365,#12366,#6488,.T.);
#15348=EDGE_CURVE('',#12366,#12367,#6489,.T.);
#15349=EDGE_CURVE('',#12367,#12368,#6490,.T.);
#15350=EDGE_CURVE('',#12368,#12369,#6491,.T.);
#15351=EDGE_CURVE('',#12369,#12370,#6492,.T.);
#15352=EDGE_CURVE('',#12370,#12371,#6493,.T.);
#15353=EDGE_CURVE('',#12371,#12372,#6494,.T.);
#15354=EDGE_CURVE('',#12372,#12373,#6495,.T.);
#15355=EDGE_CURVE('',#12373,#12374,#6496,.T.);
#15356=EDGE_CURVE('',#12374,#12131,#6497,.T.);
#15357=EDGE_CURVE('',#12375,#12130,#6498,.T.);
#15358=EDGE_CURVE('',#12375,#12376,#6499,.T.);
#15359=EDGE_CURVE('',#12376,#12377,#6500,.T.);
#15360=EDGE_CURVE('',#12378,#12377,#6501,.T.);
#15361=EDGE_CURVE('',#12378,#12379,#6502,.T.);
#15362=EDGE_CURVE('',#12379,#12380,#6503,.T.);
#15363=EDGE_CURVE('',#12380,#12381,#6504,.T.);
#15364=EDGE_CURVE('',#12381,#12382,#6505,.T.);
#15365=EDGE_CURVE('',#12382,#12383,#6506,.T.);
#15366=EDGE_CURVE('',#12383,#12384,#6507,.T.);
#15367=EDGE_CURVE('',#12384,#12385,#6508,.T.);
#15368=EDGE_CURVE('',#12385,#12386,#6509,.T.);
#15369=EDGE_CURVE('',#12386,#12387,#6510,.T.);
#15370=EDGE_CURVE('',#12387,#12388,#6511,.T.);
#15371=EDGE_CURVE('',#12388,#12389,#6512,.T.);
#15372=EDGE_CURVE('',#12389,#12390,#6513,.T.);
#15373=EDGE_CURVE('',#12390,#12391,#6514,.T.);
#15374=EDGE_CURVE('',#12391,#12392,#6515,.T.);
#15375=EDGE_CURVE('',#12392,#12139,#6516,.T.);
#15376=EDGE_CURVE('',#12393,#12138,#6517,.T.);
#15377=EDGE_CURVE('',#12393,#12394,#6518,.T.);
#15378=EDGE_CURVE('',#12394,#12395,#6519,.T.);
#15379=EDGE_CURVE('',#12396,#12395,#6520,.T.);
#15380=EDGE_CURVE('',#12396,#12397,#6521,.T.);
#15381=EDGE_CURVE('',#12397,#12398,#6522,.T.);
#15382=EDGE_CURVE('',#12398,#12399,#6523,.T.);
#15383=EDGE_CURVE('',#12399,#12400,#6524,.T.);
#15384=EDGE_CURVE('',#12400,#12401,#6525,.T.);
#15385=EDGE_CURVE('',#12401,#12402,#6526,.T.);
#15386=EDGE_CURVE('',#12402,#12403,#6527,.T.);
#15387=EDGE_CURVE('',#12403,#12404,#6528,.T.);
#15388=EDGE_CURVE('',#12404,#12405,#6529,.T.);
#15389=EDGE_CURVE('',#12405,#12406,#6530,.T.);
#15390=EDGE_CURVE('',#12406,#12407,#6531,.T.);
#15391=EDGE_CURVE('',#12407,#12408,#6532,.T.);
#15392=EDGE_CURVE('',#12408,#12409,#6533,.T.);
#15393=EDGE_CURVE('',#12409,#12410,#6534,.T.);
#15394=EDGE_CURVE('',#12410,#12147,#6535,.T.);
#15395=EDGE_CURVE('',#12411,#12146,#6536,.T.);
#15396=EDGE_CURVE('',#12411,#12412,#6537,.T.);
#15397=EDGE_CURVE('',#12412,#12413,#6538,.T.);
#15398=EDGE_CURVE('',#12414,#12413,#6539,.T.);
#15399=EDGE_CURVE('',#12414,#12415,#6540,.T.);
#15400=EDGE_CURVE('',#12415,#12416,#6541,.T.);
#15401=EDGE_CURVE('',#12416,#12417,#6542,.T.);
#15402=EDGE_CURVE('',#12417,#12418,#6543,.T.);
#15403=EDGE_CURVE('',#12418,#12419,#6544,.T.);
#15404=EDGE_CURVE('',#12419,#12420,#6545,.T.);
#15405=EDGE_CURVE('',#12420,#12421,#6546,.T.);
#15406=EDGE_CURVE('',#12421,#12422,#6547,.T.);
#15407=EDGE_CURVE('',#12422,#12423,#6548,.T.);
#15408=EDGE_CURVE('',#12423,#12424,#6549,.T.);
#15409=EDGE_CURVE('',#12424,#12425,#6550,.T.);
#15410=EDGE_CURVE('',#12425,#12426,#6551,.T.);
#15411=EDGE_CURVE('',#12426,#12427,#6552,.T.);
#15412=EDGE_CURVE('',#12427,#12428,#6553,.T.);
#15413=EDGE_CURVE('',#12428,#12155,#6554,.T.);
#15414=EDGE_CURVE('',#12429,#12154,#6555,.T.);
#15415=EDGE_CURVE('',#12429,#12430,#6556,.T.);
#15416=EDGE_CURVE('',#12430,#12431,#6557,.T.);
#15417=EDGE_CURVE('',#12432,#12431,#6558,.T.);
#15418=EDGE_CURVE('',#12432,#12433,#6559,.T.);
#15419=EDGE_CURVE('',#12433,#12434,#6560,.T.);
#15420=EDGE_CURVE('',#12434,#12435,#6561,.T.);
#15421=EDGE_CURVE('',#12435,#12436,#6562,.T.);
#15422=EDGE_CURVE('',#12436,#12437,#6563,.T.);
#15423=EDGE_CURVE('',#12437,#12438,#6564,.T.);
#15424=EDGE_CURVE('',#12438,#12439,#6565,.T.);
#15425=EDGE_CURVE('',#12439,#12440,#6566,.T.);
#15426=EDGE_CURVE('',#12440,#12441,#6567,.T.);
#15427=EDGE_CURVE('',#12441,#12442,#6568,.T.);
#15428=EDGE_CURVE('',#12442,#12443,#6569,.T.);
#15429=EDGE_CURVE('',#12443,#12444,#6570,.T.);
#15430=EDGE_CURVE('',#12444,#12445,#6571,.T.);
#15431=EDGE_CURVE('',#12445,#12446,#6572,.T.);
#15432=EDGE_CURVE('',#12446,#12163,#6573,.T.);
#15433=EDGE_CURVE('',#12447,#12162,#6574,.T.);
#15434=EDGE_CURVE('',#12447,#12448,#6575,.T.);
#15435=EDGE_CURVE('',#12448,#12449,#6576,.T.);
#15436=EDGE_CURVE('',#12450,#12449,#6577,.T.);
#15437=EDGE_CURVE('',#12450,#12451,#6578,.T.);
#15438=EDGE_CURVE('',#12451,#12452,#6579,.T.);
#15439=EDGE_CURVE('',#12452,#12453,#6580,.T.);
#15440=EDGE_CURVE('',#12453,#12454,#6581,.T.);
#15441=EDGE_CURVE('',#12454,#12455,#6582,.T.);
#15442=EDGE_CURVE('',#12455,#12456,#6583,.T.);
#15443=EDGE_CURVE('',#12456,#12457,#6584,.T.);
#15444=EDGE_CURVE('',#12457,#12458,#6585,.T.);
#15445=EDGE_CURVE('',#12458,#12459,#6586,.T.);
#15446=EDGE_CURVE('',#12459,#12460,#6587,.T.);
#15447=EDGE_CURVE('',#12460,#12461,#6588,.T.);
#15448=EDGE_CURVE('',#12461,#12462,#6589,.T.);
#15449=EDGE_CURVE('',#12462,#12463,#6590,.T.);
#15450=EDGE_CURVE('',#12463,#12464,#6591,.T.);
#15451=EDGE_CURVE('',#12464,#12171,#6592,.T.);
#15452=EDGE_CURVE('',#12465,#12170,#6593,.T.);
#15453=EDGE_CURVE('',#12465,#12466,#6594,.T.);
#15454=EDGE_CURVE('',#12466,#12467,#6595,.T.);
#15455=EDGE_CURVE('',#12468,#12467,#6596,.T.);
#15456=EDGE_CURVE('',#12468,#12469,#6597,.T.);
#15457=EDGE_CURVE('',#12469,#12470,#6598,.T.);
#15458=EDGE_CURVE('',#12470,#12471,#6599,.T.);
#15459=EDGE_CURVE('',#12471,#12472,#6600,.T.);
#15460=EDGE_CURVE('',#12472,#12473,#6601,.T.);
#15461=EDGE_CURVE('',#12473,#12474,#6602,.T.);
#15462=EDGE_CURVE('',#12474,#12475,#6603,.T.);
#15463=EDGE_CURVE('',#12475,#12476,#6604,.T.);
#15464=EDGE_CURVE('',#12476,#12477,#6605,.T.);
#15465=EDGE_CURVE('',#12477,#12478,#6606,.T.);
#15466=EDGE_CURVE('',#12478,#12479,#6607,.T.);
#15467=EDGE_CURVE('',#12479,#12480,#6608,.T.);
#15468=EDGE_CURVE('',#12480,#12481,#6609,.T.);
#15469=EDGE_CURVE('',#12481,#12482,#6610,.T.);
#15470=EDGE_CURVE('',#12482,#12179,#6611,.T.);
#15471=EDGE_CURVE('',#12483,#12483,#10578,.T.);
#15472=EDGE_CURVE('',#12484,#12468,#6612,.T.);
#15473=EDGE_CURVE('',#12467,#12263,#6613,.F.);
#15474=EDGE_CURVE('',#12264,#12484,#6614,.T.);
#15475=EDGE_CURVE('',#12172,#12485,#6615,.T.);
#15476=EDGE_CURVE('',#12485,#12486,#6616,.T.);
#15477=EDGE_CURVE('',#12486,#12465,#6617,.F.);
#15478=EDGE_CURVE('',#12487,#12450,#6618,.T.);
#15479=EDGE_CURVE('',#12449,#12256,#6619,.F.);
#15480=EDGE_CURVE('',#12257,#12487,#6620,.T.);
#15481=EDGE_CURVE('',#12164,#12488,#6621,.T.);
#15482=EDGE_CURVE('',#12488,#12489,#6622,.T.);
#15483=EDGE_CURVE('',#12489,#12447,#6623,.F.);
#15484=EDGE_CURVE('',#12490,#12432,#6624,.T.);
#15485=EDGE_CURVE('',#12431,#12249,#6625,.F.);
#15486=EDGE_CURVE('',#12250,#12490,#6626,.T.);
#15487=EDGE_CURVE('',#12156,#12491,#6627,.T.);
#15488=EDGE_CURVE('',#12491,#12492,#6628,.T.);
#15489=EDGE_CURVE('',#12492,#12429,#6629,.F.);
#15490=EDGE_CURVE('',#12493,#12414,#6630,.T.);
#15491=EDGE_CURVE('',#12413,#12242,#6631,.F.);
#15492=EDGE_CURVE('',#12243,#12493,#6632,.T.);
#15493=EDGE_CURVE('',#12148,#12494,#6633,.T.);
#15494=EDGE_CURVE('',#12494,#12495,#6634,.T.);
#15495=EDGE_CURVE('',#12495,#12411,#6635,.F.);
#15496=EDGE_CURVE('',#12496,#12396,#6636,.T.);
#15497=EDGE_CURVE('',#12395,#12235,#6637,.F.);
#15498=EDGE_CURVE('',#12236,#12496,#6638,.T.);
#15499=EDGE_CURVE('',#12140,#12497,#6639,.T.);
#15500=EDGE_CURVE('',#12497,#12498,#6640,.T.);
#15501=EDGE_CURVE('',#12498,#12393,#6641,.F.);
#15502=EDGE_CURVE('',#12499,#12378,#6642,.T.);
#15503=EDGE_CURVE('',#12377,#12228,#6643,.F.);
#15504=EDGE_CURVE('',#12229,#12499,#6644,.T.);
#15505=EDGE_CURVE('',#12132,#12500,#6645,.T.);
#15506=EDGE_CURVE('',#12500,#12501,#6646,.T.);
#15507=EDGE_CURVE('',#12501,#12375,#6647,.F.);
#15508=EDGE_CURVE('',#12502,#12360,#6648,.T.);
#15509=EDGE_CURVE('',#12359,#12221,#6649,.F.);
#15510=EDGE_CURVE('',#12222,#12502,#6650,.T.);
#15511=EDGE_CURVE('',#12124,#12503,#6651,.T.);
#15512=EDGE_CURVE('',#12503,#12504,#6652,.T.);
#15513=EDGE_CURVE('',#12504,#12357,#6653,.F.);
#15514=EDGE_CURVE('',#12505,#12342,#6654,.T.);
#15515=EDGE_CURVE('',#12341,#12214,#6655,.F.);
#15516=EDGE_CURVE('',#12215,#12505,#6656,.T.);
#15517=EDGE_CURVE('',#12116,#12506,#6657,.T.);
#15518=EDGE_CURVE('',#12506,#12507,#6658,.T.);
#15519=EDGE_CURVE('',#12507,#12339,#6659,.F.);
#15520=EDGE_CURVE('',#12508,#12324,#6660,.T.);
#15521=EDGE_CURVE('',#12323,#12207,#6661,.F.);
#15522=EDGE_CURVE('',#12208,#12508,#6662,.T.);
#15523=EDGE_CURVE('',#12108,#12509,#6663,.T.);
#15524=EDGE_CURVE('',#12509,#12510,#6664,.T.);
#15525=EDGE_CURVE('',#12510,#12321,#6665,.F.);
#15526=EDGE_CURVE('',#12511,#12306,#6666,.T.);
#15527=EDGE_CURVE('',#12305,#12200,#6667,.F.);
#15528=EDGE_CURVE('',#12201,#12511,#6668,.T.);
#15529=EDGE_CURVE('',#12100,#12512,#6669,.T.);
#15530=EDGE_CURVE('',#12512,#12513,#6670,.T.);
#15531=EDGE_CURVE('',#12513,#12303,#6671,.F.);
#15532=EDGE_CURVE('',#12514,#12288,#6672,.T.);
#15533=EDGE_CURVE('',#12287,#12193,#6673,.F.);
#15534=EDGE_CURVE('',#12194,#12514,#6674,.T.);
#15535=EDGE_CURVE('',#12092,#12515,#6675,.T.);
#15536=EDGE_CURVE('',#12515,#12516,#6676,.T.);
#15537=EDGE_CURVE('',#12516,#12285,#6677,.F.);
#15538=EDGE_CURVE('',#12517,#12270,#6678,.T.);
#15539=EDGE_CURVE('',#12269,#12186,#6679,.F.);
#15540=EDGE_CURVE('',#12187,#12517,#6680,.T.);
#15541=EDGE_CURVE('',#11868,#12268,#6681,.T.);
#15542=EDGE_CURVE('',#12174,#12266,#6682,.T.);
#15543=EDGE_CURVE('',#12175,#12265,#6683,.T.);
#15544=EDGE_CURVE('',#11872,#12482,#6684,.T.);
#15545=EDGE_CURVE('',#11873,#12481,#6685,.T.);
#15546=EDGE_CURVE('',#11874,#12480,#6686,.T.);
#15547=EDGE_CURVE('',#11875,#12479,#6687,.T.);
#15548=EDGE_CURVE('',#11876,#12478,#6688,.T.);
#15549=EDGE_CURVE('',#11877,#12477,#6689,.T.);
#15550=EDGE_CURVE('',#11878,#12476,#6690,.T.);
#15551=EDGE_CURVE('',#11879,#12475,#6691,.T.);
#15552=EDGE_CURVE('',#11880,#12474,#6692,.T.);
#15553=EDGE_CURVE('',#11881,#12473,#6693,.T.);
#15554=EDGE_CURVE('',#11882,#12472,#6694,.T.);
#15555=EDGE_CURVE('',#11883,#12471,#6695,.T.);
#15556=EDGE_CURVE('',#11884,#12470,#6696,.T.);
#15557=EDGE_CURVE('',#11885,#12469,#6697,.T.);
#15558=EDGE_CURVE('',#12261,#12484,#6698,.T.);
#15559=EDGE_CURVE('',#11888,#12466,#6699,.T.);
#15560=EDGE_CURVE('',#12166,#12486,#6700,.T.);
#15561=EDGE_CURVE('',#12167,#12485,#6701,.T.);
#15562=EDGE_CURVE('',#11892,#12464,#6702,.T.);
#15563=EDGE_CURVE('',#11893,#12463,#6703,.T.);
#15564=EDGE_CURVE('',#11894,#12462,#6704,.T.);
#15565=EDGE_CURVE('',#11895,#12461,#6705,.T.);
#15566=EDGE_CURVE('',#11896,#12460,#6706,.T.);
#15567=EDGE_CURVE('',#11897,#12459,#6707,.T.);
#15568=EDGE_CURVE('',#11898,#12458,#6708,.T.);
#15569=EDGE_CURVE('',#11899,#12457,#6709,.T.);
#15570=EDGE_CURVE('',#11900,#12456,#6710,.T.);
#15571=EDGE_CURVE('',#11901,#12455,#6711,.T.);
#15572=EDGE_CURVE('',#11902,#12454,#6712,.T.);
#15573=EDGE_CURVE('',#11903,#12453,#6713,.T.);
#15574=EDGE_CURVE('',#11904,#12452,#6714,.T.);
#15575=EDGE_CURVE('',#11905,#12451,#6715,.T.);
#15576=EDGE_CURVE('',#12254,#12487,#6716,.T.);
#15577=EDGE_CURVE('',#11908,#12448,#6717,.T.);
#15578=EDGE_CURVE('',#12158,#12489,#6718,.T.);
#15579=EDGE_CURVE('',#12159,#12488,#6719,.T.);
#15580=EDGE_CURVE('',#11912,#12446,#6720,.T.);
#15581=EDGE_CURVE('',#11913,#12445,#6721,.T.);
#15582=EDGE_CURVE('',#11914,#12444,#6722,.T.);
#15583=EDGE_CURVE('',#11915,#12443,#6723,.T.);
#15584=EDGE_CURVE('',#11916,#12442,#6724,.T.);
#15585=EDGE_CURVE('',#11917,#12441,#6725,.T.);
#15586=EDGE_CURVE('',#11918,#12440,#6726,.T.);
#15587=EDGE_CURVE('',#11919,#12439,#6727,.T.);
#15588=EDGE_CURVE('',#11920,#12438,#6728,.T.);
#15589=EDGE_CURVE('',#11921,#12437,#6729,.T.);
#15590=EDGE_CURVE('',#11922,#12436,#6730,.T.);
#15591=EDGE_CURVE('',#11923,#12435,#6731,.T.);
#15592=EDGE_CURVE('',#11924,#12434,#6732,.T.);
#15593=EDGE_CURVE('',#11925,#12433,#6733,.T.);
#15594=EDGE_CURVE('',#12247,#12490,#6734,.T.);
#15595=EDGE_CURVE('',#11928,#12430,#6735,.T.);
#15596=EDGE_CURVE('',#12150,#12492,#6736,.T.);
#15597=EDGE_CURVE('',#12151,#12491,#6737,.T.);
#15598=EDGE_CURVE('',#11932,#12428,#6738,.T.);
#15599=EDGE_CURVE('',#11933,#12427,#6739,.T.);
#15600=EDGE_CURVE('',#11934,#12426,#6740,.T.);
#15601=EDGE_CURVE('',#11935,#12425,#6741,.T.);
#15602=EDGE_CURVE('',#11936,#12424,#6742,.T.);
#15603=EDGE_CURVE('',#11937,#12423,#6743,.T.);
#15604=EDGE_CURVE('',#11938,#12422,#6744,.T.);
#15605=EDGE_CURVE('',#11939,#12421,#6745,.T.);
#15606=EDGE_CURVE('',#11940,#12420,#6746,.T.);
#15607=EDGE_CURVE('',#11941,#12419,#6747,.T.);
#15608=EDGE_CURVE('',#11942,#12418,#6748,.T.);
#15609=EDGE_CURVE('',#11943,#12417,#6749,.T.);
#15610=EDGE_CURVE('',#11944,#12416,#6750,.T.);
#15611=EDGE_CURVE('',#11945,#12415,#6751,.T.);
#15612=EDGE_CURVE('',#12240,#12493,#6752,.T.);
#15613=EDGE_CURVE('',#11948,#12412,#6753,.T.);
#15614=EDGE_CURVE('',#12142,#12495,#6754,.T.);
#15615=EDGE_CURVE('',#12143,#12494,#6755,.T.);
#15616=EDGE_CURVE('',#11952,#12410,#6756,.T.);
#15617=EDGE_CURVE('',#11953,#12409,#6757,.T.);
#15618=EDGE_CURVE('',#11954,#12408,#6758,.T.);
#15619=EDGE_CURVE('',#11955,#12407,#6759,.T.);
#15620=EDGE_CURVE('',#11956,#12406,#6760,.T.);
#15621=EDGE_CURVE('',#11957,#12405,#6761,.T.);
#15622=EDGE_CURVE('',#11958,#12404,#6762,.T.);
#15623=EDGE_CURVE('',#11959,#12403,#6763,.T.);
#15624=EDGE_CURVE('',#11960,#12402,#6764,.T.);
#15625=EDGE_CURVE('',#11961,#12401,#6765,.T.);
#15626=EDGE_CURVE('',#11962,#12400,#6766,.T.);
#15627=EDGE_CURVE('',#11963,#12399,#6767,.T.);
#15628=EDGE_CURVE('',#11964,#12398,#6768,.T.);
#15629=EDGE_CURVE('',#11965,#12397,#6769,.T.);
#15630=EDGE_CURVE('',#12233,#12496,#6770,.T.);
#15631=EDGE_CURVE('',#11968,#12394,#6771,.T.);
#15632=EDGE_CURVE('',#12134,#12498,#6772,.T.);
#15633=EDGE_CURVE('',#12135,#12497,#6773,.T.);
#15634=EDGE_CURVE('',#11972,#12392,#6774,.T.);
#15635=EDGE_CURVE('',#11973,#12391,#6775,.T.);
#15636=EDGE_CURVE('',#11974,#12390,#6776,.T.);
#15637=EDGE_CURVE('',#11975,#12389,#6777,.T.);
#15638=EDGE_CURVE('',#11976,#12388,#6778,.T.);
#15639=EDGE_CURVE('',#11977,#12387,#6779,.T.);
#15640=EDGE_CURVE('',#11978,#12386,#6780,.T.);
#15641=EDGE_CURVE('',#11979,#12385,#6781,.T.);
#15642=EDGE_CURVE('',#11980,#12384,#6782,.T.);
#15643=EDGE_CURVE('',#11981,#12383,#6783,.T.);
#15644=EDGE_CURVE('',#11982,#12382,#6784,.T.);
#15645=EDGE_CURVE('',#11983,#12381,#6785,.T.);
#15646=EDGE_CURVE('',#11984,#12380,#6786,.T.);
#15647=EDGE_CURVE('',#11985,#12379,#6787,.T.);
#15648=EDGE_CURVE('',#12226,#12499,#6788,.T.);
#15649=EDGE_CURVE('',#11988,#12376,#6789,.T.);
#15650=EDGE_CURVE('',#12126,#12501,#6790,.T.);
#15651=EDGE_CURVE('',#12127,#12500,#6791,.T.);
#15652=EDGE_CURVE('',#11992,#12374,#6792,.T.);
#15653=EDGE_CURVE('',#11993,#12373,#6793,.T.);
#15654=EDGE_CURVE('',#11994,#12372,#6794,.T.);
#15655=EDGE_CURVE('',#11995,#12371,#6795,.T.);
#15656=EDGE_CURVE('',#11996,#12370,#6796,.T.);
#15657=EDGE_CURVE('',#11997,#12369,#6797,.T.);
#15658=EDGE_CURVE('',#11998,#12368,#6798,.T.);
#15659=EDGE_CURVE('',#11999,#12367,#6799,.T.);
#15660=EDGE_CURVE('',#12000,#12366,#6800,.T.);
#15661=EDGE_CURVE('',#12001,#12365,#6801,.T.);
#15662=EDGE_CURVE('',#12002,#12364,#6802,.T.);
#15663=EDGE_CURVE('',#12003,#12363,#6803,.T.);
#15664=EDGE_CURVE('',#12004,#12362,#6804,.T.);
#15665=EDGE_CURVE('',#12005,#12361,#6805,.T.);
#15666=EDGE_CURVE('',#12219,#12502,#6806,.T.);
#15667=EDGE_CURVE('',#12008,#12358,#6807,.T.);
#15668=EDGE_CURVE('',#12118,#12504,#6808,.T.);
#15669=EDGE_CURVE('',#12119,#12503,#6809,.T.);
#15670=EDGE_CURVE('',#12012,#12356,#6810,.T.);
#15671=EDGE_CURVE('',#12013,#12355,#6811,.T.);
#15672=EDGE_CURVE('',#12014,#12354,#6812,.T.);
#15673=EDGE_CURVE('',#12015,#12353,#6813,.T.);
#15674=EDGE_CURVE('',#12016,#12352,#6814,.T.);
#15675=EDGE_CURVE('',#12017,#12351,#6815,.T.);
#15676=EDGE_CURVE('',#12018,#12350,#6816,.T.);
#15677=EDGE_CURVE('',#12019,#12349,#6817,.T.);
#15678=EDGE_CURVE('',#12020,#12348,#6818,.T.);
#15679=EDGE_CURVE('',#12021,#12347,#6819,.T.);
#15680=EDGE_CURVE('',#12022,#12346,#6820,.T.);
#15681=EDGE_CURVE('',#12023,#12345,#6821,.T.);
#15682=EDGE_CURVE('',#12024,#12344,#6822,.T.);
#15683=EDGE_CURVE('',#12025,#12343,#6823,.T.);
#15684=EDGE_CURVE('',#12212,#12505,#6824,.T.);
#15685=EDGE_CURVE('',#12028,#12340,#6825,.T.);
#15686=EDGE_CURVE('',#12110,#12507,#6826,.T.);
#15687=EDGE_CURVE('',#12111,#12506,#6827,.T.);
#15688=EDGE_CURVE('',#12032,#12338,#6828,.T.);
#15689=EDGE_CURVE('',#12033,#12337,#6829,.T.);
#15690=EDGE_CURVE('',#12034,#12336,#6830,.T.);
#15691=EDGE_CURVE('',#12035,#12335,#6831,.T.);
#15692=EDGE_CURVE('',#12036,#12334,#6832,.T.);
#15693=EDGE_CURVE('',#12037,#12333,#6833,.T.);
#15694=EDGE_CURVE('',#12038,#12332,#6834,.T.);
#15695=EDGE_CURVE('',#12039,#12331,#6835,.T.);
#15696=EDGE_CURVE('',#12040,#12330,#6836,.T.);
#15697=EDGE_CURVE('',#12041,#12329,#6837,.T.);
#15698=EDGE_CURVE('',#12042,#12328,#6838,.T.);
#15699=EDGE_CURVE('',#12043,#12327,#6839,.T.);
#15700=EDGE_CURVE('',#12044,#12326,#6840,.T.);
#15701=EDGE_CURVE('',#12045,#12325,#6841,.T.);
#15702=EDGE_CURVE('',#12205,#12508,#6842,.T.);
#15703=EDGE_CURVE('',#12048,#12322,#6843,.T.);
#15704=EDGE_CURVE('',#12102,#12510,#6844,.T.);
#15705=EDGE_CURVE('',#12103,#12509,#6845,.T.);
#15706=EDGE_CURVE('',#12052,#12320,#6846,.T.);
#15707=EDGE_CURVE('',#12053,#12319,#6847,.T.);
#15708=EDGE_CURVE('',#12054,#12318,#6848,.T.);
#15709=EDGE_CURVE('',#12055,#12317,#6849,.T.);
#15710=EDGE_CURVE('',#12056,#12316,#6850,.T.);
#15711=EDGE_CURVE('',#12057,#12315,#6851,.T.);
#15712=EDGE_CURVE('',#12058,#12314,#6852,.T.);
#15713=EDGE_CURVE('',#12059,#12313,#6853,.T.);
#15714=EDGE_CURVE('',#12060,#12312,#6854,.T.);
#15715=EDGE_CURVE('',#12061,#12311,#6855,.T.);
#15716=EDGE_CURVE('',#12062,#12310,#6856,.T.);
#15717=EDGE_CURVE('',#12063,#12309,#6857,.T.);
#15718=EDGE_CURVE('',#12064,#12308,#6858,.T.);
#15719=EDGE_CURVE('',#12065,#12307,#6859,.T.);
#15720=EDGE_CURVE('',#12198,#12511,#6860,.T.);
#15721=EDGE_CURVE('',#12068,#12304,#6861,.T.);
#15722=EDGE_CURVE('',#12094,#12513,#6862,.T.);
#15723=EDGE_CURVE('',#12095,#12512,#6863,.T.);
#15724=EDGE_CURVE('',#12072,#12302,#6864,.T.);
#15725=EDGE_CURVE('',#12073,#12301,#6865,.T.);
#15726=EDGE_CURVE('',#12074,#12300,#6866,.T.);
#15727=EDGE_CURVE('',#12075,#12299,#6867,.T.);
#15728=EDGE_CURVE('',#12076,#12298,#6868,.T.);
#15729=EDGE_CURVE('',#12077,#12297,#6869,.T.);
#15730=EDGE_CURVE('',#12078,#12296,#6870,.T.);
#15731=EDGE_CURVE('',#12079,#12295,#6871,.T.);
#15732=EDGE_CURVE('',#12080,#12294,#6872,.T.);
#15733=EDGE_CURVE('',#12081,#12293,#6873,.T.);
#15734=EDGE_CURVE('',#12082,#12292,#6874,.T.);
#15735=EDGE_CURVE('',#12083,#12291,#6875,.T.);
#15736=EDGE_CURVE('',#12084,#12290,#6876,.T.);
#15737=EDGE_CURVE('',#12085,#12289,#6877,.T.);
#15738=EDGE_CURVE('',#12191,#12514,#6878,.T.);
#15739=EDGE_CURVE('',#11850,#12286,#6879,.T.);
#15740=EDGE_CURVE('',#11847,#12516,#6880,.T.);
#15741=EDGE_CURVE('',#11848,#12515,#6881,.T.);
#15742=EDGE_CURVE('',#11852,#12284,#6882,.T.);
#15743=EDGE_CURVE('',#11853,#12283,#6883,.T.);
#15744=EDGE_CURVE('',#11854,#12282,#6884,.T.);
#15745=EDGE_CURVE('',#11855,#12281,#6885,.T.);
#15746=EDGE_CURVE('',#11856,#12280,#6886,.T.);
#15747=EDGE_CURVE('',#11857,#12279,#6887,.T.);
#15748=EDGE_CURVE('',#11858,#12278,#6888,.T.);
#15749=EDGE_CURVE('',#11859,#12277,#6889,.T.);
#15750=EDGE_CURVE('',#11860,#12276,#6890,.T.);
#15751=EDGE_CURVE('',#11861,#12275,#6891,.T.);
#15752=EDGE_CURVE('',#11862,#12274,#6892,.T.);
#15753=EDGE_CURVE('',#11863,#12273,#6893,.T.);
#15754=EDGE_CURVE('',#11864,#12272,#6894,.T.);
#15755=EDGE_CURVE('',#11865,#12271,#6895,.T.);
#15756=EDGE_CURVE('',#12184,#12517,#6896,.T.);
#15757=EDGE_CURVE('',#12088,#12518,#6897,.T.);
#15758=EDGE_CURVE('',#12518,#12518,#10579,.T.);
#15759=EDGE_CURVE('',#12519,#12519,#10580,.T.);
#15760=EDGE_CURVE('',#12519,#12483,#6898,.T.);
#15761=EDGE_CURVE('',#12520,#12521,#6899,.T.);
#15762=EDGE_CURVE('',#12520,#12522,#6900,.T.);
#15763=EDGE_CURVE('',#12522,#12523,#6901,.T.);
#15764=EDGE_CURVE('',#12521,#12523,#6902,.T.);
#15765=EDGE_CURVE('',#12524,#12520,#6903,.T.);
#15766=EDGE_CURVE('',#12524,#12525,#6904,.T.);
#15767=EDGE_CURVE('',#12525,#12522,#6905,.T.);
#15768=EDGE_CURVE('',#12526,#12524,#6906,.T.);
#15769=EDGE_CURVE('',#12526,#12527,#6907,.T.);
#15770=EDGE_CURVE('',#12527,#12525,#6908,.T.);
#15771=EDGE_CURVE('',#12521,#12526,#6909,.T.);
#15772=EDGE_CURVE('',#12523,#12527,#6910,.T.);
#15773=EDGE_CURVE('',#12528,#12529,#6911,.T.);
#15774=EDGE_CURVE('',#12528,#12530,#6912,.T.);
#15775=EDGE_CURVE('',#12530,#12531,#6913,.T.);
#15776=EDGE_CURVE('',#12529,#12531,#6914,.T.);
#15777=EDGE_CURVE('',#12532,#12528,#6915,.T.);
#15778=EDGE_CURVE('',#12532,#12533,#6916,.T.);
#15779=EDGE_CURVE('',#12533,#12530,#6917,.T.);
#15780=EDGE_CURVE('',#12534,#12532,#6918,.T.);
#15781=EDGE_CURVE('',#12534,#12535,#6919,.T.);
#15782=EDGE_CURVE('',#12535,#12533,#6920,.T.);
#15783=EDGE_CURVE('',#12529,#12534,#6921,.T.);
#15784=EDGE_CURVE('',#12531,#12535,#6922,.T.);
#15785=EDGE_CURVE('',#12536,#12536,#10581,.T.);
#15786=EDGE_CURVE('',#12536,#12537,#6923,.T.);
#15787=EDGE_CURVE('',#12537,#12537,#10582,.T.);
#15788=EDGE_CURVE('',#12538,#12538,#10583,.T.);
#15789=EDGE_CURVE('',#12538,#12539,#6924,.T.);
#15790=EDGE_CURVE('',#12539,#12539,#10584,.T.);
#15791=EDGE_CURVE('',#12540,#12541,#10585,.T.);
#15792=EDGE_CURVE('',#12541,#12542,#6925,.T.);
#15793=EDGE_CURVE('',#12543,#12542,#10586,.T.);
#15794=EDGE_CURVE('',#12540,#12543,#6926,.T.);
#15795=EDGE_CURVE('',#12541,#12540,#10587,.T.);
#15796=EDGE_CURVE('',#12542,#12543,#10588,.T.);
#15797=EDGE_CURVE('',#12544,#12545,#10589,.T.);
#15798=EDGE_CURVE('',#12545,#12544,#10590,.T.);
#15799=EDGE_CURVE('',#12544,#12546,#6927,.T.);
#15800=EDGE_CURVE('',#12546,#12546,#10591,.T.);
#15801=EDGE_CURVE('',#12547,#12547,#10592,.T.);
#15802=EDGE_CURVE('',#12548,#12548,#10593,.T.);
#15803=EDGE_CURVE('',#12548,#12545,#6928,.T.);
#15804=EDGE_CURVE('',#12549,#12549,#10594,.T.);
#15805=EDGE_CURVE('',#12549,#12547,#6929,.T.);
#15806=EDGE_CURVE('',#12550,#12550,#10595,.T.);
#15807=EDGE_CURVE('',#12551,#12551,#10596,.T.);
#15808=EDGE_CURVE('',#12551,#12550,#6930,.T.);
#15809=EDGE_CURVE('',#12552,#12552,#10597,.T.);
#15810=EDGE_CURVE('',#12552,#12553,#6931,.T.);
#15811=EDGE_CURVE('',#12553,#12553,#10598,.T.);
#15812=EDGE_CURVE('',#12554,#12554,#10599,.T.);
#15813=EDGE_CURVE('',#12554,#12549,#6932,.T.);
#15814=EDGE_CURVE('',#12555,#12556,#6933,.T.);
#15815=EDGE_CURVE('',#12556,#12557,#111,.T.);
#15816=EDGE_CURVE('',#12557,#12558,#6934,.T.);
#15817=EDGE_CURVE('',#12558,#12555,#297,.T.);
#15818=EDGE_CURVE('',#12559,#12555,#10600,.T.);
#15819=EDGE_CURVE('',#12558,#12560,#10601,.T.);
#15820=EDGE_CURVE('',#12560,#12559,#298,.T.);
#15821=EDGE_CURVE('',#12560,#12561,#6935,.T.);
#15822=EDGE_CURVE('',#12561,#12562,#112,.T.);
#15823=EDGE_CURVE('',#12562,#12559,#6936,.T.);
#15824=EDGE_CURVE('',#12563,#12555,#6937,.T.);
#15825=EDGE_CURVE('',#12564,#12563,#6938,.T.);
#15826=EDGE_CURVE('',#12564,#12556,#6939,.T.);
#15827=EDGE_CURVE('',#12565,#12559,#6940,.T.);
#15828=EDGE_CURVE('',#12563,#12565,#10602,.T.);
#15829=EDGE_CURVE('',#12566,#12562,#6941,.T.);
#15830=EDGE_CURVE('',#12565,#12566,#6942,.T.);
#15831=EDGE_CURVE('',#12566,#12567,#113,.T.);
#15832=EDGE_CURVE('',#12567,#12568,#6943,.T.);
#15833=EDGE_CURVE('',#12568,#12565,#299,.T.);
#15834=EDGE_CURVE('',#12568,#12569,#10603,.T.);
#15835=EDGE_CURVE('',#12569,#12563,#300,.T.);
#15836=EDGE_CURVE('',#12569,#12570,#6944,.T.);
#15837=EDGE_CURVE('',#12570,#12564,#114,.T.);
#15838=EDGE_CURVE('',#12570,#12567,#10604,.T.);
#15839=EDGE_CURVE('',#12571,#12571,#10605,.T.);
#15840=EDGE_CURVE('',#12572,#12572,#10606,.T.);
#15841=EDGE_CURVE('',#12557,#12561,#10607,.T.);
#15842=EDGE_CURVE('',#12571,#12573,#6945,.T.);
#15843=EDGE_CURVE('',#12573,#12573,#10608,.T.);
#15844=EDGE_CURVE('',#12573,#12574,#6946,.T.);
#15845=EDGE_CURVE('',#12574,#12574,#10609,.T.);
#15846=EDGE_CURVE('',#12575,#12575,#10610,.T.);
#15847=EDGE_CURVE('',#12575,#12574,#6947,.T.);
#15848=EDGE_CURVE('',#12576,#12576,#10611,.T.);
#15849=EDGE_CURVE('',#12572,#12577,#6948,.T.);
#15850=EDGE_CURVE('',#12577,#12577,#10612,.T.);
#15851=EDGE_CURVE('',#12577,#12578,#6949,.T.);
#15852=EDGE_CURVE('',#12578,#12578,#10613,.T.);
#15853=EDGE_CURVE('',#12576,#12578,#6950,.T.);
#15854=EDGE_CURVE('',#12579,#12580,#6951,.T.);
#15855=EDGE_CURVE('',#12580,#12581,#6952,.T.);
#15856=EDGE_CURVE('',#12581,#12582,#6953,.T.);
#15857=EDGE_CURVE('',#12582,#12583,#6954,.T.);
#15858=EDGE_CURVE('',#12583,#12584,#6955,.T.);
#15859=EDGE_CURVE('',#12584,#12579,#6956,.T.);
#15860=EDGE_CURVE('',#12585,#12583,#6957,.T.);
#15861=EDGE_CURVE('',#12586,#12585,#6958,.T.);
#15862=EDGE_CURVE('',#12584,#12586,#6959,.T.);
#15863=EDGE_CURVE('',#12587,#12582,#6960,.T.);
#15864=EDGE_CURVE('',#12587,#12588,#6961,.T.);
#15865=EDGE_CURVE('',#12589,#12588,#6962,.T.);
#15866=EDGE_CURVE('',#12585,#12589,#6963,.T.);
#15867=EDGE_CURVE('',#12581,#12590,#6964,.T.);
#15868=EDGE_CURVE('',#12591,#12590,#6965,.T.);
#15869=EDGE_CURVE('',#12591,#12592,#6966,.T.);
#15870=EDGE_CURVE('',#12592,#12587,#6967,.T.);
#15871=EDGE_CURVE('',#12590,#12593,#6968,.T.);
#15872=EDGE_CURVE('',#12593,#12594,#6969,.T.);
#15873=EDGE_CURVE('',#12594,#12595,#6970,.T.);
#15874=EDGE_CURVE('',#12595,#12596,#6971,.T.);
#15875=EDGE_CURVE('',#12596,#12591,#6972,.T.);
#15876=EDGE_CURVE('',#12597,#12595,#6973,.T.);
#15877=EDGE_CURVE('',#12598,#12597,#6974,.T.);
#15878=EDGE_CURVE('',#12596,#12598,#6975,.T.);
#15879=EDGE_CURVE('',#12599,#12594,#6976,.T.);
#15880=EDGE_CURVE('',#12599,#12600,#6977,.T.);
#15881=EDGE_CURVE('',#12601,#12600,#6978,.T.);
#15882=EDGE_CURVE('',#12597,#12601,#6979,.T.);
#15883=EDGE_CURVE('',#12579,#12602,#6980,.T.);
#15884=EDGE_CURVE('',#12602,#12599,#6981,.T.);
#15885=EDGE_CURVE('',#12593,#12580,#6982,.T.);
#15886=EDGE_CURVE('',#12603,#12592,#6983,.T.);
#15887=EDGE_CURVE('',#12588,#12603,#6984,.T.);
#15888=EDGE_CURVE('',#12601,#12604,#6985,.T.);
#15889=EDGE_CURVE('',#12604,#12605,#6986,.T.);
#15890=EDGE_CURVE('',#12605,#12606,#6987,.T.);
#15891=EDGE_CURVE('',#12606,#12598,#6988,.T.);
#15892=EDGE_CURVE('',#12605,#12607,#6989,.T.);
#15893=EDGE_CURVE('',#12607,#12589,#6990,.T.);
#15894=EDGE_CURVE('',#12603,#12606,#6991,.T.);
#15895=EDGE_CURVE('',#12608,#12604,#6992,.T.);
#15896=EDGE_CURVE('',#12607,#12608,#6993,.T.);
#15897=EDGE_CURVE('',#12600,#12609,#6994,.T.);
#15898=EDGE_CURVE('',#12609,#12610,#6995,.T.);
#15899=EDGE_CURVE('',#12608,#12610,#6996,.T.);
#15900=EDGE_CURVE('',#12610,#12586,#6997,.T.);
#15901=EDGE_CURVE('',#12609,#12602,#6998,.T.);
#15902=EDGE_CURVE('',#12611,#12612,#10614,.T.);
#15903=EDGE_CURVE('',#12612,#12611,#10615,.T.);
#15904=EDGE_CURVE('',#12612,#12613,#10616,.T.);
#15905=EDGE_CURVE('',#12613,#12614,#10617,.T.);
#15906=EDGE_CURVE('',#12614,#12613,#10618,.T.);
#15907=EDGE_CURVE('',#12614,#12615,#6999,.T.);
#15908=EDGE_CURVE('',#12615,#12616,#10619,.T.);
#15909=EDGE_CURVE('',#12616,#12615,#10620,.T.);
#15910=EDGE_CURVE('',#12616,#12617,#10621,.T.);
#15911=EDGE_CURVE('',#12617,#12618,#10622,.T.);
#15912=EDGE_CURVE('',#12618,#12617,#10623,.T.);
#15913=EDGE_CURVE('',#12618,#12611,#7000,.T.);
#15914=EDGE_CURVE('',#12619,#12620,#7001,.T.);
#15915=EDGE_CURVE('',#12621,#12619,#7002,.T.);
#15916=EDGE_CURVE('',#12620,#12621,#7003,.T.);
#15917=EDGE_CURVE('',#12622,#12623,#7004,.T.);
#15918=EDGE_CURVE('',#12624,#12622,#7005,.T.);
#15919=EDGE_CURVE('',#12623,#12624,#7006,.T.);
#15920=EDGE_CURVE('',#12625,#12626,#7007,.T.);
#15921=EDGE_CURVE('',#12627,#12625,#7008,.T.);
#15922=EDGE_CURVE('',#12626,#12627,#7009,.T.);
#15923=EDGE_CURVE('',#12628,#12629,#7010,.T.);
#15924=EDGE_CURVE('',#12630,#12628,#7011,.T.);
#15925=EDGE_CURVE('',#12629,#12630,#7012,.T.);
#15926=EDGE_CURVE('',#12628,#12624,#7013,.T.);
#15927=EDGE_CURVE('',#12622,#12630,#7014,.T.);
#15928=EDGE_CURVE('',#12631,#12632,#7015,.T.);
#15929=EDGE_CURVE('',#12633,#12631,#7016,.T.);
#15930=EDGE_CURVE('',#12632,#12633,#7017,.T.);
#15931=EDGE_CURVE('',#12634,#12635,#7018,.T.);
#15932=EDGE_CURVE('',#12636,#12634,#7019,.T.);
#15933=EDGE_CURVE('',#12635,#12636,#7020,.T.);
#15934=EDGE_CURVE('',#12634,#12629,#7021,.T.);
#15935=EDGE_CURVE('',#12630,#12636,#7022,.T.);
#15936=EDGE_CURVE('',#12631,#12635,#7023,.T.);
#15937=EDGE_CURVE('',#12636,#12633,#7024,.T.);
#15938=EDGE_CURVE('',#12637,#12638,#123,.T.);
#15939=EDGE_CURVE('',#12638,#12634,#7025,.T.);
#15940=EDGE_CURVE('',#12635,#12637,#7026,.T.);
#15941=EDGE_CURVE('',#12625,#12632,#7027,.T.);
#15942=EDGE_CURVE('',#12633,#12627,#7028,.T.);
#15943=EDGE_CURVE('',#12639,#12640,#124,.T.);
#15944=EDGE_CURVE('',#12640,#12631,#7029,.T.);
#15945=EDGE_CURVE('',#12632,#12639,#7030,.T.);
#15946=EDGE_CURVE('',#12641,#12642,#125,.T.);
#15947=EDGE_CURVE('',#12642,#12628,#7031,.T.);
#15948=EDGE_CURVE('',#12629,#12641,#7032,.T.);
#15949=EDGE_CURVE('',#12619,#12626,#7033,.T.);
#15950=EDGE_CURVE('',#12627,#12621,#7034,.T.);
#15951=EDGE_CURVE('',#12643,#12644,#126,.T.);
#15952=EDGE_CURVE('',#12644,#12625,#7035,.T.);
#15953=EDGE_CURVE('',#12626,#12643,#7036,.T.);
#15954=EDGE_CURVE('',#12645,#12646,#127,.T.);
#15955=EDGE_CURVE('',#12646,#12623,#7037,.T.);
#15956=EDGE_CURVE('',#12624,#12645,#7038,.T.);
#15957=EDGE_CURVE('',#12623,#12620,#7039,.T.);
#15958=EDGE_CURVE('',#12621,#12622,#7040,.T.);
#15959=EDGE_CURVE('',#12647,#12648,#128,.T.);
#15960=EDGE_CURVE('',#12648,#12619,#7041,.T.);
#15961=EDGE_CURVE('',#12620,#12647,#7042,.T.);
#15962=EDGE_CURVE('',#12640,#12637,#129,.T.);
#15963=EDGE_CURVE('',#12644,#12649,#130,.T.);
#15964=EDGE_CURVE('',#12649,#12639,#131,.T.);
#15965=EDGE_CURVE('',#12648,#12643,#132,.T.);
#15966=EDGE_CURVE('',#12650,#12650,#10624,.T.);
#15967=EDGE_CURVE('',#12651,#12652,#7043,.T.);
#15968=EDGE_CURVE('',#12652,#12653,#7044,.T.);
#15969=EDGE_CURVE('',#12653,#12654,#7045,.T.);
#15970=EDGE_CURVE('',#12651,#12654,#7046,.T.);
#15971=EDGE_CURVE('',#12652,#12655,#7047,.T.);
#15972=EDGE_CURVE('',#12655,#12656,#7048,.T.);
#15973=EDGE_CURVE('',#12656,#12653,#7049,.T.);
#15974=EDGE_CURVE('',#12657,#12658,#7050,.T.);
#15975=EDGE_CURVE('',#12658,#12659,#7051,.T.);
#15976=EDGE_CURVE('',#12659,#12660,#7052,.T.);
#15977=EDGE_CURVE('',#12660,#12657,#7053,.T.);
#15978=EDGE_CURVE('',#12661,#12659,#7054,.T.);
#15979=EDGE_CURVE('',#12658,#12662,#7055,.T.);
#15980=EDGE_CURVE('',#12662,#12661,#7056,.T.);
#15981=EDGE_CURVE('',#12655,#12657,#7057,.T.);
#15982=EDGE_CURVE('',#12660,#12656,#7058,.T.);
#15983=EDGE_CURVE('',#12654,#12661,#7059,.T.);
#15984=EDGE_CURVE('',#12662,#12651,#7060,.T.);
#15985=EDGE_CURVE('',#12656,#12663,#7061,.T.);
#15986=EDGE_CURVE('',#12663,#12664,#7062,.T.);
#15987=EDGE_CURVE('',#12653,#12664,#7063,.T.);
#15988=EDGE_CURVE('',#12660,#12665,#7064,.T.);
#15989=EDGE_CURVE('',#12665,#12663,#7065,.T.);
#15990=EDGE_CURVE('',#12659,#12666,#7066,.T.);
#15991=EDGE_CURVE('',#12666,#12665,#7067,.T.);
#15992=EDGE_CURVE('',#12667,#12667,#10625,.T.);
#15993=EDGE_CURVE('',#12661,#12668,#7068,.T.);
#15994=EDGE_CURVE('',#12668,#12666,#7069,.T.);
#15995=EDGE_CURVE('',#12654,#12669,#7070,.T.);
#15996=EDGE_CURVE('',#12669,#12668,#7071,.T.);
#15997=EDGE_CURVE('',#12664,#12669,#7072,.T.);
#15998=EDGE_CURVE('',#12649,#12667,#7073,.T.);
#15999=EDGE_CURVE('',#12646,#12647,#133,.T.);
#16000=EDGE_CURVE('',#12642,#12645,#134,.T.);
#16001=EDGE_CURVE('',#12638,#12641,#135,.T.);
#16002=EDGE_CURVE('',#12670,#12670,#10626,.T.);
#16003=EDGE_CURVE('',#12671,#12671,#10627,.T.);
#16004=EDGE_CURVE('',#12671,#12670,#7074,.T.);
#16005=EDGE_CURVE('',#12672,#12672,#10628,.T.);
#16006=EDGE_CURVE('',#12672,#12671,#7075,.T.);
#16007=EDGE_CURVE('',#12673,#12673,#10629,.T.);
#16008=EDGE_CURVE('',#12650,#12673,#7076,.T.);
#16009=EDGE_CURVE('',#12674,#12674,#10630,.T.);
#16010=EDGE_CURVE('',#12674,#12675,#7077,.T.);
#16011=EDGE_CURVE('',#12675,#12675,#10631,.T.);
#16012=EDGE_CURVE('',#12676,#12676,#10632,.T.);
#16013=EDGE_CURVE('',#12677,#12677,#10633,.T.);
#16014=EDGE_CURVE('',#12678,#12678,#10634,.T.);
#16015=EDGE_CURVE('',#12678,#12677,#7078,.T.);
#16016=EDGE_CURVE('',#12679,#12679,#10635,.T.);
#16017=EDGE_CURVE('',#12679,#12680,#7079,.T.);
#16018=EDGE_CURVE('',#12680,#12680,#10636,.T.);
#16019=EDGE_CURVE('',#12681,#12681,#10637,.T.);
#16020=EDGE_CURVE('',#12682,#12682,#10638,.T.);
#16021=EDGE_CURVE('',#12682,#12681,#7080,.T.);
#16022=EDGE_CURVE('',#12683,#12683,#10639,.T.);
#16023=EDGE_CURVE('',#12683,#12684,#7081,.T.);
#16024=EDGE_CURVE('',#12684,#12684,#10640,.T.);
#16025=EDGE_CURVE('',#12676,#12685,#7082,.T.);
#16026=EDGE_CURVE('',#12685,#12685,#10641,.T.);
#16027=EDGE_CURVE('',#12686,#12687,#7083,.T.);
#16028=EDGE_CURVE('',#12686,#12688,#301,.T.);
#16029=EDGE_CURVE('',#12688,#12689,#10642,.T.);
#16030=EDGE_CURVE('',#12689,#12687,#302,.T.);
#16031=EDGE_CURVE('',#12690,#12691,#7084,.T.);
#16032=EDGE_CURVE('',#12690,#12686,#303,.T.);
#16033=EDGE_CURVE('',#12687,#12691,#304,.T.);
#16034=EDGE_CURVE('',#12692,#12693,#7085,.T.);
#16035=EDGE_CURVE('',#12692,#12690,#305,.T.);
#16036=EDGE_CURVE('',#12691,#12693,#306,.T.);
#16037=EDGE_CURVE('',#12694,#12695,#7086,.T.);
#16038=EDGE_CURVE('',#12694,#12692,#307,.T.);
#16039=EDGE_CURVE('',#12693,#12695,#308,.T.);
#16040=EDGE_CURVE('',#12696,#12697,#7087,.T.);
#16041=EDGE_CURVE('',#12696,#12694,#309,.T.);
#16042=EDGE_CURVE('',#12695,#12697,#310,.T.);
#16043=EDGE_CURVE('',#12698,#12699,#7088,.T.);
#16044=EDGE_CURVE('',#12698,#12696,#311,.T.);
#16045=EDGE_CURVE('',#12697,#12699,#312,.T.);
#16046=EDGE_CURVE('',#12700,#12701,#7089,.T.);
#16047=EDGE_CURVE('',#12700,#12698,#313,.T.);
#16048=EDGE_CURVE('',#12699,#12701,#314,.T.);
#16049=EDGE_CURVE('',#12702,#12703,#7090,.T.);
#16050=EDGE_CURVE('',#12702,#12700,#315,.T.);
#16051=EDGE_CURVE('',#12701,#12703,#316,.T.);
#16052=EDGE_CURVE('',#12704,#12705,#7091,.T.);
#16053=EDGE_CURVE('',#12704,#12702,#317,.T.);
#16054=EDGE_CURVE('',#12703,#12705,#318,.T.);
#16055=EDGE_CURVE('',#12706,#12707,#7092,.T.);
#16056=EDGE_CURVE('',#12706,#12704,#319,.T.);
#16057=EDGE_CURVE('',#12705,#12707,#320,.T.);
#16058=EDGE_CURVE('',#12708,#12709,#7093,.T.);
#16059=EDGE_CURVE('',#12708,#12706,#321,.T.);
#16060=EDGE_CURVE('',#12707,#12709,#322,.T.);
#16061=EDGE_CURVE('',#12710,#12711,#7094,.T.);
#16062=EDGE_CURVE('',#12710,#12708,#323,.T.);
#16063=EDGE_CURVE('',#12709,#12711,#324,.T.);
#16064=EDGE_CURVE('',#12712,#12713,#7095,.T.);
#16065=EDGE_CURVE('',#12712,#12710,#325,.T.);
#16066=EDGE_CURVE('',#12711,#12713,#326,.T.);
#16067=EDGE_CURVE('',#12714,#12715,#7096,.T.);
#16068=EDGE_CURVE('',#12714,#12712,#327,.T.);
#16069=EDGE_CURVE('',#12713,#12715,#328,.T.);
#16070=EDGE_CURVE('',#12716,#12717,#7097,.T.);
#16071=EDGE_CURVE('',#12716,#12714,#329,.T.);
#16072=EDGE_CURVE('',#12715,#12717,#330,.T.);
#16073=EDGE_CURVE('',#12718,#12719,#7098,.T.);
#16074=EDGE_CURVE('',#12718,#12716,#331,.T.);
#16075=EDGE_CURVE('',#12717,#12719,#332,.T.);
#16076=EDGE_CURVE('',#12720,#12721,#7099,.T.);
#16077=EDGE_CURVE('',#12720,#12718,#333,.T.);
#16078=EDGE_CURVE('',#12719,#12721,#334,.T.);
#16079=EDGE_CURVE('',#12722,#12723,#7100,.T.);
#16080=EDGE_CURVE('',#12722,#12720,#335,.T.);
#16081=EDGE_CURVE('',#12721,#12723,#336,.T.);
#16082=EDGE_CURVE('',#12724,#12725,#7101,.T.);
#16083=EDGE_CURVE('',#12724,#12722,#337,.T.);
#16084=EDGE_CURVE('',#12723,#12725,#338,.T.);
#16085=EDGE_CURVE('',#12726,#12727,#7102,.T.);
#16086=EDGE_CURVE('',#12726,#12724,#339,.T.);
#16087=EDGE_CURVE('',#12725,#12727,#340,.T.);
#16088=EDGE_CURVE('',#12728,#12729,#7103,.T.);
#16089=EDGE_CURVE('',#12730,#12728,#10643,.F.);
#16090=EDGE_CURVE('',#12730,#12726,#341,.T.);
#16091=EDGE_CURVE('',#12727,#12729,#342,.T.);
#16092=EDGE_CURVE('',#12731,#12732,#7104,.T.);
#16093=EDGE_CURVE('',#12731,#12733,#343,.T.);
#16094=EDGE_CURVE('',#12734,#12733,#10644,.T.);
#16095=EDGE_CURVE('',#12732,#12734,#344,.T.);
#16096=EDGE_CURVE('',#12735,#12736,#7105,.T.);
#16097=EDGE_CURVE('',#12735,#12731,#345,.T.);
#16098=EDGE_CURVE('',#12736,#12732,#346,.T.);
#16099=EDGE_CURVE('',#12737,#12738,#7106,.T.);
#16100=EDGE_CURVE('',#12737,#12735,#347,.T.);
#16101=EDGE_CURVE('',#12738,#12736,#348,.T.);
#16102=EDGE_CURVE('',#12739,#12740,#7107,.T.);
#16103=EDGE_CURVE('',#12739,#12737,#349,.T.);
#16104=EDGE_CURVE('',#12740,#12738,#350,.T.);
#16105=EDGE_CURVE('',#12741,#12742,#7108,.T.);
#16106=EDGE_CURVE('',#12741,#12739,#351,.T.);
#16107=EDGE_CURVE('',#12742,#12740,#352,.T.);
#16108=EDGE_CURVE('',#12743,#12744,#7109,.T.);
#16109=EDGE_CURVE('',#12743,#12741,#353,.T.);
#16110=EDGE_CURVE('',#12744,#12742,#354,.T.);
#16111=EDGE_CURVE('',#12745,#12746,#7110,.T.);
#16112=EDGE_CURVE('',#12745,#12743,#355,.T.);
#16113=EDGE_CURVE('',#12746,#12744,#356,.T.);
#16114=EDGE_CURVE('',#12747,#12748,#7111,.T.);
#16115=EDGE_CURVE('',#12747,#12745,#357,.T.);
#16116=EDGE_CURVE('',#12748,#12746,#358,.T.);
#16117=EDGE_CURVE('',#12749,#12750,#7112,.T.);
#16118=EDGE_CURVE('',#12749,#12747,#359,.T.);
#16119=EDGE_CURVE('',#12750,#12748,#360,.T.);
#16120=EDGE_CURVE('',#12751,#12752,#7113,.T.);
#16121=EDGE_CURVE('',#12751,#12749,#361,.T.);
#16122=EDGE_CURVE('',#12752,#12750,#362,.T.);
#16123=EDGE_CURVE('',#12753,#12754,#7114,.T.);
#16124=EDGE_CURVE('',#12753,#12751,#363,.T.);
#16125=EDGE_CURVE('',#12754,#12752,#364,.T.);
#16126=EDGE_CURVE('',#12755,#12756,#7115,.T.);
#16127=EDGE_CURVE('',#12755,#12753,#365,.T.);
#16128=EDGE_CURVE('',#12756,#12754,#366,.T.);
#16129=EDGE_CURVE('',#12757,#12758,#7116,.T.);
#16130=EDGE_CURVE('',#12757,#12755,#367,.T.);
#16131=EDGE_CURVE('',#12758,#12756,#368,.T.);
#16132=EDGE_CURVE('',#12759,#12760,#7117,.T.);
#16133=EDGE_CURVE('',#12759,#12757,#369,.T.);
#16134=EDGE_CURVE('',#12760,#12758,#370,.T.);
#16135=EDGE_CURVE('',#12761,#12762,#7118,.T.);
#16136=EDGE_CURVE('',#12761,#12759,#371,.T.);
#16137=EDGE_CURVE('',#12762,#12760,#372,.T.);
#16138=EDGE_CURVE('',#12763,#12764,#7119,.T.);
#16139=EDGE_CURVE('',#12763,#12761,#373,.T.);
#16140=EDGE_CURVE('',#12764,#12762,#374,.T.);
#16141=EDGE_CURVE('',#12765,#12766,#7120,.T.);
#16142=EDGE_CURVE('',#12765,#12763,#375,.T.);
#16143=EDGE_CURVE('',#12766,#12764,#376,.T.);
#16144=EDGE_CURVE('',#12767,#12768,#7121,.T.);
#16145=EDGE_CURVE('',#12767,#12765,#377,.T.);
#16146=EDGE_CURVE('',#12768,#12766,#378,.T.);
#16147=EDGE_CURVE('',#12769,#12770,#7122,.T.);
#16148=EDGE_CURVE('',#12769,#12767,#379,.T.);
#16149=EDGE_CURVE('',#12770,#12768,#380,.T.);
#16150=EDGE_CURVE('',#12771,#12772,#7123,.T.);
#16151=EDGE_CURVE('',#12771,#12769,#381,.T.);
#16152=EDGE_CURVE('',#12772,#12770,#382,.T.);
#16153=EDGE_CURVE('',#12733,#12730,#383,.T.);
#16154=EDGE_CURVE('',#12773,#12730,#10645,.F.);
#16155=EDGE_CURVE('',#12773,#12734,#384,.T.);
#16156=EDGE_CURVE('',#12729,#12773,#385,.T.);
#16157=EDGE_CURVE('',#12774,#12689,#386,.T.);
#16158=EDGE_CURVE('',#12774,#12772,#387,.T.);
#16159=EDGE_CURVE('',#12689,#12775,#10646,.T.);
#16160=EDGE_CURVE('',#12775,#12688,#10647,.T.);
#16161=EDGE_CURVE('',#12688,#12776,#388,.T.);
#16162=EDGE_CURVE('',#12776,#12774,#10648,.T.);
#16163=EDGE_CURVE('',#12776,#12771,#389,.T.);
#16164=EDGE_CURVE('',#12777,#12778,#7124,.T.);
#16165=EDGE_CURVE('',#12777,#12779,#7125,.T.);
#16166=EDGE_CURVE('',#12780,#12779,#7126,.T.);
#16167=EDGE_CURVE('',#12778,#12780,#7127,.T.);
#16168=EDGE_CURVE('',#12778,#12781,#10649,.T.);
#16169=EDGE_CURVE('',#12780,#12781,#7128,.T.);
#16170=EDGE_CURVE('',#12781,#12782,#7129,.T.);
#16171=EDGE_CURVE('',#12779,#12782,#7130,.T.);
#16172=EDGE_CURVE('',#12782,#12777,#10650,.T.);
#16173=EDGE_CURVE('',#12783,#12784,#7131,.T.);
#16174=EDGE_CURVE('',#12783,#12785,#7132,.T.);
#16175=EDGE_CURVE('',#12786,#12785,#7133,.T.);
#16176=EDGE_CURVE('',#12784,#12786,#7134,.T.);
#16177=EDGE_CURVE('',#12784,#12787,#10651,.T.);
#16178=EDGE_CURVE('',#12786,#12787,#7135,.T.);
#16179=EDGE_CURVE('',#12787,#12788,#7136,.T.);
#16180=EDGE_CURVE('',#12785,#12788,#7137,.T.);
#16181=EDGE_CURVE('',#12788,#12783,#10652,.T.);
#16182=EDGE_CURVE('',#12789,#12790,#7138,.T.);
#16183=EDGE_CURVE('',#12789,#12791,#7139,.T.);
#16184=EDGE_CURVE('',#12792,#12791,#7140,.T.);
#16185=EDGE_CURVE('',#12790,#12792,#7141,.T.);
#16186=EDGE_CURVE('',#12790,#12793,#10653,.T.);
#16187=EDGE_CURVE('',#12792,#12793,#7142,.T.);
#16188=EDGE_CURVE('',#12793,#12794,#7143,.T.);
#16189=EDGE_CURVE('',#12791,#12794,#7144,.T.);
#16190=EDGE_CURVE('',#12794,#12789,#10654,.T.);
#16191=EDGE_CURVE('',#12795,#12796,#7145,.T.);
#16192=EDGE_CURVE('',#12795,#12797,#7146,.T.);
#16193=EDGE_CURVE('',#12798,#12797,#7147,.T.);
#16194=EDGE_CURVE('',#12796,#12798,#7148,.T.);
#16195=EDGE_CURVE('',#12796,#12799,#10655,.T.);
#16196=EDGE_CURVE('',#12798,#12799,#7149,.T.);
#16197=EDGE_CURVE('',#12799,#12800,#7150,.T.);
#16198=EDGE_CURVE('',#12797,#12800,#7151,.T.);
#16199=EDGE_CURVE('',#12800,#12795,#10656,.T.);
#16200=EDGE_CURVE('',#12801,#12802,#7152,.T.);
#16201=EDGE_CURVE('',#12801,#12803,#7153,.T.);
#16202=EDGE_CURVE('',#12804,#12803,#7154,.T.);
#16203=EDGE_CURVE('',#12802,#12804,#7155,.T.);
#16204=EDGE_CURVE('',#12802,#12805,#10657,.T.);
#16205=EDGE_CURVE('',#12804,#12805,#7156,.T.);
#16206=EDGE_CURVE('',#12805,#12806,#7157,.T.);
#16207=EDGE_CURVE('',#12803,#12806,#7158,.T.);
#16208=EDGE_CURVE('',#12806,#12801,#10658,.T.);
#16209=EDGE_CURVE('',#12807,#12808,#7159,.T.);
#16210=EDGE_CURVE('',#12807,#12809,#7160,.T.);
#16211=EDGE_CURVE('',#12810,#12809,#7161,.T.);
#16212=EDGE_CURVE('',#12808,#12810,#7162,.T.);
#16213=EDGE_CURVE('',#12808,#12811,#10659,.T.);
#16214=EDGE_CURVE('',#12810,#12811,#7163,.T.);
#16215=EDGE_CURVE('',#12811,#12812,#7164,.T.);
#16216=EDGE_CURVE('',#12809,#12812,#7165,.T.);
#16217=EDGE_CURVE('',#12812,#12807,#10660,.T.);
#16218=EDGE_CURVE('',#12813,#12814,#7166,.T.);
#16219=EDGE_CURVE('',#12813,#12815,#7167,.T.);
#16220=EDGE_CURVE('',#12816,#12815,#7168,.T.);
#16221=EDGE_CURVE('',#12814,#12816,#7169,.T.);
#16222=EDGE_CURVE('',#12814,#12817,#10661,.T.);
#16223=EDGE_CURVE('',#12816,#12817,#7170,.T.);
#16224=EDGE_CURVE('',#12817,#12818,#7171,.T.);
#16225=EDGE_CURVE('',#12815,#12818,#7172,.T.);
#16226=EDGE_CURVE('',#12818,#12813,#10662,.T.);
#16227=EDGE_CURVE('',#12819,#12820,#7173,.T.);
#16228=EDGE_CURVE('',#12819,#12821,#7174,.T.);
#16229=EDGE_CURVE('',#12822,#12821,#7175,.T.);
#16230=EDGE_CURVE('',#12820,#12822,#7176,.T.);
#16231=EDGE_CURVE('',#12820,#12823,#10663,.T.);
#16232=EDGE_CURVE('',#12822,#12823,#7177,.T.);
#16233=EDGE_CURVE('',#12823,#12824,#7178,.T.);
#16234=EDGE_CURVE('',#12821,#12824,#7179,.T.);
#16235=EDGE_CURVE('',#12824,#12819,#10664,.T.);
#16236=EDGE_CURVE('',#12825,#12826,#7180,.T.);
#16237=EDGE_CURVE('',#12825,#12827,#7181,.T.);
#16238=EDGE_CURVE('',#12828,#12827,#7182,.T.);
#16239=EDGE_CURVE('',#12826,#12828,#7183,.T.);
#16240=EDGE_CURVE('',#12826,#12829,#10665,.T.);
#16241=EDGE_CURVE('',#12828,#12829,#7184,.T.);
#16242=EDGE_CURVE('',#12829,#12830,#7185,.T.);
#16243=EDGE_CURVE('',#12827,#12830,#7186,.T.);
#16244=EDGE_CURVE('',#12830,#12825,#10666,.T.);
#16245=EDGE_CURVE('',#12831,#12832,#7187,.T.);
#16246=EDGE_CURVE('',#12831,#12833,#7188,.T.);
#16247=EDGE_CURVE('',#12834,#12833,#7189,.T.);
#16248=EDGE_CURVE('',#12832,#12834,#7190,.T.);
#16249=EDGE_CURVE('',#12832,#12835,#10667,.T.);
#16250=EDGE_CURVE('',#12834,#12835,#7191,.T.);
#16251=EDGE_CURVE('',#12835,#12836,#7192,.T.);
#16252=EDGE_CURVE('',#12833,#12836,#7193,.T.);
#16253=EDGE_CURVE('',#12836,#12831,#10668,.T.);
#16254=EDGE_CURVE('',#12837,#12838,#7194,.T.);
#16255=EDGE_CURVE('',#12837,#12839,#7195,.T.);
#16256=EDGE_CURVE('',#12840,#12839,#7196,.T.);
#16257=EDGE_CURVE('',#12838,#12840,#7197,.T.);
#16258=EDGE_CURVE('',#12838,#12841,#10669,.T.);
#16259=EDGE_CURVE('',#12840,#12841,#7198,.T.);
#16260=EDGE_CURVE('',#12841,#12842,#7199,.T.);
#16261=EDGE_CURVE('',#12839,#12842,#7200,.T.);
#16262=EDGE_CURVE('',#12842,#12837,#10670,.T.);
#16263=EDGE_CURVE('',#12843,#12844,#7201,.T.);
#16264=EDGE_CURVE('',#12843,#12845,#7202,.T.);
#16265=EDGE_CURVE('',#12846,#12845,#7203,.T.);
#16266=EDGE_CURVE('',#12844,#12846,#7204,.T.);
#16267=EDGE_CURVE('',#12844,#12847,#10671,.T.);
#16268=EDGE_CURVE('',#12846,#12847,#7205,.T.);
#16269=EDGE_CURVE('',#12847,#12848,#7206,.T.);
#16270=EDGE_CURVE('',#12845,#12848,#7207,.T.);
#16271=EDGE_CURVE('',#12848,#12843,#10672,.T.);
#16272=EDGE_CURVE('',#12849,#12850,#7208,.T.);
#16273=EDGE_CURVE('',#12849,#12851,#7209,.T.);
#16274=EDGE_CURVE('',#12852,#12851,#7210,.T.);
#16275=EDGE_CURVE('',#12850,#12852,#7211,.T.);
#16276=EDGE_CURVE('',#12850,#12853,#10673,.T.);
#16277=EDGE_CURVE('',#12852,#12853,#7212,.T.);
#16278=EDGE_CURVE('',#12853,#12854,#7213,.T.);
#16279=EDGE_CURVE('',#12851,#12854,#7214,.T.);
#16280=EDGE_CURVE('',#12854,#12849,#10674,.T.);
#16281=EDGE_CURVE('',#12855,#12856,#7215,.T.);
#16282=EDGE_CURVE('',#12855,#12857,#7216,.T.);
#16283=EDGE_CURVE('',#12858,#12857,#7217,.T.);
#16284=EDGE_CURVE('',#12856,#12858,#7218,.T.);
#16285=EDGE_CURVE('',#12856,#12859,#10675,.T.);
#16286=EDGE_CURVE('',#12858,#12859,#7219,.T.);
#16287=EDGE_CURVE('',#12859,#12860,#7220,.T.);
#16288=EDGE_CURVE('',#12857,#12860,#7221,.T.);
#16289=EDGE_CURVE('',#12860,#12855,#10676,.T.);
#16290=EDGE_CURVE('',#12861,#12862,#7222,.T.);
#16291=EDGE_CURVE('',#12861,#12863,#7223,.T.);
#16292=EDGE_CURVE('',#12864,#12863,#7224,.T.);
#16293=EDGE_CURVE('',#12862,#12864,#7225,.T.);
#16294=EDGE_CURVE('',#12862,#12865,#10677,.T.);
#16295=EDGE_CURVE('',#12864,#12865,#7226,.T.);
#16296=EDGE_CURVE('',#12865,#12866,#7227,.T.);
#16297=EDGE_CURVE('',#12863,#12866,#7228,.T.);
#16298=EDGE_CURVE('',#12866,#12861,#10678,.T.);
#16299=EDGE_CURVE('',#12867,#12868,#7229,.T.);
#16300=EDGE_CURVE('',#12867,#12869,#7230,.T.);
#16301=EDGE_CURVE('',#12870,#12869,#7231,.T.);
#16302=EDGE_CURVE('',#12868,#12870,#7232,.T.);
#16303=EDGE_CURVE('',#12868,#12871,#10679,.T.);
#16304=EDGE_CURVE('',#12870,#12871,#7233,.T.);
#16305=EDGE_CURVE('',#12871,#12872,#7234,.T.);
#16306=EDGE_CURVE('',#12869,#12872,#7235,.T.);
#16307=EDGE_CURVE('',#12872,#12867,#10680,.T.);
#16308=EDGE_CURVE('',#12873,#12874,#7236,.T.);
#16309=EDGE_CURVE('',#12873,#12875,#7237,.T.);
#16310=EDGE_CURVE('',#12876,#12875,#7238,.T.);
#16311=EDGE_CURVE('',#12874,#12876,#7239,.T.);
#16312=EDGE_CURVE('',#12874,#12877,#10681,.T.);
#16313=EDGE_CURVE('',#12876,#12877,#7240,.T.);
#16314=EDGE_CURVE('',#12877,#12878,#7241,.T.);
#16315=EDGE_CURVE('',#12875,#12878,#7242,.T.);
#16316=EDGE_CURVE('',#12878,#12873,#10682,.T.);
#16317=EDGE_CURVE('',#12879,#12880,#7243,.T.);
#16318=EDGE_CURVE('',#12879,#12881,#7244,.T.);
#16319=EDGE_CURVE('',#12882,#12881,#7245,.T.);
#16320=EDGE_CURVE('',#12880,#12882,#7246,.T.);
#16321=EDGE_CURVE('',#12880,#12883,#10683,.T.);
#16322=EDGE_CURVE('',#12882,#12884,#7247,.T.);
#16323=EDGE_CURVE('',#12883,#12884,#10684,.T.);
#16324=EDGE_CURVE('',#12884,#12885,#7248,.T.);
#16325=EDGE_CURVE('',#12881,#12885,#7249,.T.);
#16326=EDGE_CURVE('',#12885,#12886,#10685,.T.);
#16327=EDGE_CURVE('',#12886,#12879,#10686,.T.);
#16328=EDGE_CURVE('',#12887,#12888,#7250,.T.);
#16329=EDGE_CURVE('',#12887,#12889,#7251,.T.);
#16330=EDGE_CURVE('',#12890,#12889,#7252,.T.);
#16331=EDGE_CURVE('',#12888,#12890,#7253,.T.);
#16332=EDGE_CURVE('',#12888,#12891,#10687,.T.);
#16333=EDGE_CURVE('',#12890,#12891,#7254,.T.);
#16334=EDGE_CURVE('',#12891,#12892,#7255,.T.);
#16335=EDGE_CURVE('',#12889,#12892,#7256,.T.);
#16336=EDGE_CURVE('',#12892,#12887,#10688,.T.);
#16337=EDGE_CURVE('',#12893,#12894,#7257,.T.);
#16338=EDGE_CURVE('',#12893,#12895,#7258,.T.);
#16339=EDGE_CURVE('',#12896,#12895,#7259,.T.);
#16340=EDGE_CURVE('',#12894,#12896,#7260,.T.);
#16341=EDGE_CURVE('',#12894,#12897,#10689,.T.);
#16342=EDGE_CURVE('',#12896,#12897,#7261,.T.);
#16343=EDGE_CURVE('',#12897,#12898,#7262,.T.);
#16344=EDGE_CURVE('',#12895,#12898,#7263,.T.);
#16345=EDGE_CURVE('',#12898,#12893,#10690,.T.);
#16346=EDGE_CURVE('',#12899,#12900,#7264,.T.);
#16347=EDGE_CURVE('',#12899,#12901,#7265,.T.);
#16348=EDGE_CURVE('',#12902,#12901,#7266,.T.);
#16349=EDGE_CURVE('',#12900,#12902,#7267,.T.);
#16350=EDGE_CURVE('',#12900,#12903,#10691,.T.);
#16351=EDGE_CURVE('',#12902,#12903,#7268,.T.);
#16352=EDGE_CURVE('',#12903,#12904,#7269,.T.);
#16353=EDGE_CURVE('',#12901,#12904,#7270,.T.);
#16354=EDGE_CURVE('',#12904,#12899,#10692,.T.);
#16355=EDGE_CURVE('',#12905,#12906,#7271,.T.);
#16356=EDGE_CURVE('',#12905,#12907,#7272,.T.);
#16357=EDGE_CURVE('',#12908,#12907,#7273,.T.);
#16358=EDGE_CURVE('',#12906,#12908,#7274,.T.);
#16359=EDGE_CURVE('',#12906,#12909,#10693,.T.);
#16360=EDGE_CURVE('',#12908,#12909,#7275,.T.);
#16361=EDGE_CURVE('',#12909,#12910,#7276,.T.);
#16362=EDGE_CURVE('',#12907,#12910,#7277,.T.);
#16363=EDGE_CURVE('',#12910,#12905,#10694,.T.);
#16364=EDGE_CURVE('',#12911,#12912,#7278,.T.);
#16365=EDGE_CURVE('',#12911,#12913,#7279,.T.);
#16366=EDGE_CURVE('',#12914,#12913,#7280,.T.);
#16367=EDGE_CURVE('',#12912,#12914,#7281,.T.);
#16368=EDGE_CURVE('',#12912,#12915,#10695,.T.);
#16369=EDGE_CURVE('',#12914,#12915,#7282,.T.);
#16370=EDGE_CURVE('',#12915,#12916,#7283,.T.);
#16371=EDGE_CURVE('',#12913,#12916,#7284,.T.);
#16372=EDGE_CURVE('',#12916,#12911,#10696,.T.);
#16373=EDGE_CURVE('',#12917,#12918,#7285,.T.);
#16374=EDGE_CURVE('',#12917,#12919,#7286,.T.);
#16375=EDGE_CURVE('',#12920,#12919,#7287,.T.);
#16376=EDGE_CURVE('',#12918,#12920,#7288,.T.);
#16377=EDGE_CURVE('',#12918,#12921,#10697,.T.);
#16378=EDGE_CURVE('',#12920,#12921,#7289,.T.);
#16379=EDGE_CURVE('',#12921,#12922,#7290,.T.);
#16380=EDGE_CURVE('',#12919,#12922,#7291,.T.);
#16381=EDGE_CURVE('',#12922,#12917,#10698,.T.);
#16382=EDGE_CURVE('',#12923,#12924,#7292,.T.);
#16383=EDGE_CURVE('',#12923,#12925,#7293,.T.);
#16384=EDGE_CURVE('',#12926,#12925,#7294,.T.);
#16385=EDGE_CURVE('',#12924,#12926,#7295,.T.);
#16386=EDGE_CURVE('',#12924,#12927,#10699,.T.);
#16387=EDGE_CURVE('',#12926,#12927,#7296,.T.);
#16388=EDGE_CURVE('',#12927,#12928,#7297,.T.);
#16389=EDGE_CURVE('',#12925,#12928,#7298,.T.);
#16390=EDGE_CURVE('',#12928,#12923,#10700,.T.);
#16391=EDGE_CURVE('',#12929,#12930,#7299,.T.);
#16392=EDGE_CURVE('',#12929,#12931,#7300,.T.);
#16393=EDGE_CURVE('',#12932,#12931,#7301,.T.);
#16394=EDGE_CURVE('',#12930,#12932,#7302,.T.);
#16395=EDGE_CURVE('',#12930,#12933,#10701,.T.);
#16396=EDGE_CURVE('',#12932,#12933,#7303,.T.);
#16397=EDGE_CURVE('',#12933,#12934,#7304,.T.);
#16398=EDGE_CURVE('',#12931,#12934,#7305,.T.);
#16399=EDGE_CURVE('',#12934,#12929,#10702,.T.);
#16400=EDGE_CURVE('',#12935,#12936,#7306,.T.);
#16401=EDGE_CURVE('',#12935,#12937,#7307,.T.);
#16402=EDGE_CURVE('',#12938,#12937,#7308,.T.);
#16403=EDGE_CURVE('',#12936,#12938,#7309,.T.);
#16404=EDGE_CURVE('',#12936,#12939,#10703,.T.);
#16405=EDGE_CURVE('',#12938,#12939,#7310,.T.);
#16406=EDGE_CURVE('',#12939,#12940,#7311,.T.);
#16407=EDGE_CURVE('',#12937,#12940,#7312,.T.);
#16408=EDGE_CURVE('',#12940,#12935,#10704,.T.);
#16409=EDGE_CURVE('',#12941,#12942,#7313,.T.);
#16410=EDGE_CURVE('',#12941,#12943,#7314,.T.);
#16411=EDGE_CURVE('',#12944,#12943,#7315,.T.);
#16412=EDGE_CURVE('',#12942,#12944,#7316,.T.);
#16413=EDGE_CURVE('',#12942,#12945,#10705,.T.);
#16414=EDGE_CURVE('',#12944,#12945,#7317,.T.);
#16415=EDGE_CURVE('',#12945,#12946,#7318,.T.);
#16416=EDGE_CURVE('',#12943,#12946,#7319,.T.);
#16417=EDGE_CURVE('',#12946,#12941,#10706,.T.);
#16418=EDGE_CURVE('',#12947,#12948,#7320,.T.);
#16419=EDGE_CURVE('',#12947,#12949,#7321,.T.);
#16420=EDGE_CURVE('',#12950,#12949,#7322,.T.);
#16421=EDGE_CURVE('',#12948,#12950,#7323,.T.);
#16422=EDGE_CURVE('',#12948,#12951,#10707,.T.);
#16423=EDGE_CURVE('',#12950,#12951,#7324,.T.);
#16424=EDGE_CURVE('',#12951,#12952,#7325,.T.);
#16425=EDGE_CURVE('',#12949,#12952,#7326,.T.);
#16426=EDGE_CURVE('',#12952,#12947,#10708,.T.);
#16427=EDGE_CURVE('',#12953,#12954,#7327,.T.);
#16428=EDGE_CURVE('',#12953,#12955,#7328,.T.);
#16429=EDGE_CURVE('',#12956,#12955,#7329,.T.);
#16430=EDGE_CURVE('',#12954,#12956,#7330,.T.);
#16431=EDGE_CURVE('',#12954,#12957,#10709,.T.);
#16432=EDGE_CURVE('',#12956,#12957,#7331,.T.);
#16433=EDGE_CURVE('',#12957,#12958,#7332,.T.);
#16434=EDGE_CURVE('',#12955,#12958,#7333,.T.);
#16435=EDGE_CURVE('',#12958,#12953,#10710,.T.);
#16436=EDGE_CURVE('',#12959,#12960,#7334,.T.);
#16437=EDGE_CURVE('',#12959,#12961,#7335,.T.);
#16438=EDGE_CURVE('',#12962,#12961,#7336,.T.);
#16439=EDGE_CURVE('',#12960,#12962,#7337,.T.);
#16440=EDGE_CURVE('',#12960,#12963,#10711,.T.);
#16441=EDGE_CURVE('',#12962,#12963,#7338,.T.);
#16442=EDGE_CURVE('',#12963,#12964,#7339,.T.);
#16443=EDGE_CURVE('',#12961,#12964,#7340,.T.);
#16444=EDGE_CURVE('',#12964,#12959,#10712,.T.);
#16445=EDGE_CURVE('',#12965,#12966,#7341,.T.);
#16446=EDGE_CURVE('',#12965,#12967,#7342,.T.);
#16447=EDGE_CURVE('',#12968,#12967,#7343,.T.);
#16448=EDGE_CURVE('',#12966,#12968,#7344,.T.);
#16449=EDGE_CURVE('',#12966,#12969,#10713,.T.);
#16450=EDGE_CURVE('',#12968,#12969,#7345,.T.);
#16451=EDGE_CURVE('',#12969,#12970,#7346,.T.);
#16452=EDGE_CURVE('',#12967,#12970,#7347,.T.);
#16453=EDGE_CURVE('',#12970,#12965,#10714,.T.);
#16454=EDGE_CURVE('',#12971,#12972,#7348,.T.);
#16455=EDGE_CURVE('',#12971,#12973,#7349,.T.);
#16456=EDGE_CURVE('',#12974,#12973,#7350,.T.);
#16457=EDGE_CURVE('',#12972,#12974,#7351,.T.);
#16458=EDGE_CURVE('',#12972,#12975,#10715,.T.);
#16459=EDGE_CURVE('',#12974,#12975,#7352,.T.);
#16460=EDGE_CURVE('',#12975,#12976,#7353,.T.);
#16461=EDGE_CURVE('',#12973,#12976,#7354,.T.);
#16462=EDGE_CURVE('',#12976,#12971,#10716,.T.);
#16463=EDGE_CURVE('',#12977,#12978,#7355,.T.);
#16464=EDGE_CURVE('',#12977,#12979,#7356,.T.);
#16465=EDGE_CURVE('',#12980,#12979,#7357,.T.);
#16466=EDGE_CURVE('',#12978,#12980,#7358,.T.);
#16467=EDGE_CURVE('',#12978,#12981,#10717,.T.);
#16468=EDGE_CURVE('',#12980,#12981,#7359,.T.);
#16469=EDGE_CURVE('',#12981,#12982,#7360,.T.);
#16470=EDGE_CURVE('',#12979,#12982,#7361,.T.);
#16471=EDGE_CURVE('',#12982,#12977,#10718,.T.);
#16472=EDGE_CURVE('',#12983,#12984,#7362,.T.);
#16473=EDGE_CURVE('',#12983,#12985,#7363,.T.);
#16474=EDGE_CURVE('',#12986,#12985,#7364,.T.);
#16475=EDGE_CURVE('',#12984,#12986,#7365,.T.);
#16476=EDGE_CURVE('',#12984,#12987,#10719,.T.);
#16477=EDGE_CURVE('',#12986,#12987,#7366,.T.);
#16478=EDGE_CURVE('',#12987,#12988,#7367,.T.);
#16479=EDGE_CURVE('',#12985,#12988,#7368,.T.);
#16480=EDGE_CURVE('',#12988,#12983,#10720,.T.);
#16481=EDGE_CURVE('',#12989,#12990,#7369,.T.);
#16482=EDGE_CURVE('',#12989,#12991,#7370,.T.);
#16483=EDGE_CURVE('',#12992,#12991,#7371,.T.);
#16484=EDGE_CURVE('',#12990,#12992,#7372,.T.);
#16485=EDGE_CURVE('',#12990,#12993,#10721,.T.);
#16486=EDGE_CURVE('',#12992,#12993,#7373,.T.);
#16487=EDGE_CURVE('',#12993,#12994,#7374,.T.);
#16488=EDGE_CURVE('',#12991,#12994,#7375,.T.);
#16489=EDGE_CURVE('',#12994,#12989,#10722,.T.);
#16490=EDGE_CURVE('',#12995,#12996,#7376,.T.);
#16491=EDGE_CURVE('',#12995,#12997,#7377,.T.);
#16492=EDGE_CURVE('',#12997,#12998,#7378,.T.);
#16493=EDGE_CURVE('',#12996,#12998,#7379,.T.);
#16494=EDGE_CURVE('',#12999,#12995,#7380,.T.);
#16495=EDGE_CURVE('',#12999,#13000,#7381,.T.);
#16496=EDGE_CURVE('',#13000,#12997,#7382,.T.);
#16497=EDGE_CURVE('',#13001,#12999,#7383,.T.);
#16498=EDGE_CURVE('',#13001,#13002,#7384,.T.);
#16499=EDGE_CURVE('',#13002,#13000,#7385,.T.);
#16500=EDGE_CURVE('',#13003,#13001,#7386,.T.);
#16501=EDGE_CURVE('',#13003,#13004,#7387,.T.);
#16502=EDGE_CURVE('',#13004,#13002,#7388,.T.);
#16503=EDGE_CURVE('',#13005,#13003,#7389,.T.);
#16504=EDGE_CURVE('',#13005,#13006,#7390,.T.);
#16505=EDGE_CURVE('',#13006,#13004,#7391,.T.);
#16506=EDGE_CURVE('',#12996,#13005,#7392,.T.);
#16507=EDGE_CURVE('',#12998,#13006,#7393,.T.);
#16508=EDGE_CURVE('',#13007,#13007,#10723,.T.);
#16509=EDGE_CURVE('',#12775,#13007,#7394,.T.);
#16510=EDGE_CURVE('',#12728,#12773,#10724,.F.);
#16511=EDGE_CURVE('',#13008,#13008,#10725,.T.);
#16512=EDGE_CURVE('',#13008,#12728,#7395,.T.);
#16513=EDGE_CURVE('',#13009,#13009,#10726,.T.);
#16514=EDGE_CURVE('',#13009,#13008,#7396,.T.);
#16515=EDGE_CURVE('',#13010,#13010,#10727,.T.);
#16516=EDGE_CURVE('',#13011,#13011,#10728,.T.);
#16517=EDGE_CURVE('',#13011,#12886,#7397,.T.);
#16518=EDGE_CURVE('',#12883,#13010,#7398,.T.);
#16519=EDGE_CURVE('',#13012,#13012,#10729,.T.);
#16520=EDGE_CURVE('',#13012,#13011,#7399,.T.);
#16521=EDGE_CURVE('',#13013,#13013,#10730,.T.);
#16522=EDGE_CURVE('',#13014,#13014,#10731,.T.);
#16523=EDGE_CURVE('',#13014,#13013,#7400,.T.);
#16524=EDGE_CURVE('',#13015,#13015,#10732,.T.);
#16525=EDGE_CURVE('',#13015,#13014,#7401,.T.);
#16526=EDGE_CURVE('',#13016,#13016,#10733,.T.);
#16527=EDGE_CURVE('',#13016,#13015,#7402,.T.);
#16528=ORIENTED_EDGE('',*,*,#13017,.T.);
#16529=ORIENTED_EDGE('',*,*,#13018,.T.);
#16530=ORIENTED_EDGE('',*,*,#13019,.T.);
#16531=ORIENTED_EDGE('',*,*,#13018,.F.);
#16532=ORIENTED_EDGE('',*,*,#13017,.F.);
#16533=ORIENTED_EDGE('',*,*,#13020,.F.);
#16534=ORIENTED_EDGE('',*,*,#13019,.F.);
#16535=ORIENTED_EDGE('',*,*,#13021,.T.);
#16536=ORIENTED_EDGE('',*,*,#13022,.F.);
#16537=ORIENTED_EDGE('',*,*,#13021,.F.);
#16538=ORIENTED_EDGE('',*,*,#13023,.T.);
#16539=ORIENTED_EDGE('',*,*,#13024,.T.);
#16540=ORIENTED_EDGE('',*,*,#13025,.T.);
#16541=ORIENTED_EDGE('',*,*,#13024,.F.);
#16542=ORIENTED_EDGE('',*,*,#13023,.F.);
#16543=ORIENTED_EDGE('',*,*,#13026,.F.);
#16544=ORIENTED_EDGE('',*,*,#13025,.F.);
#16545=ORIENTED_EDGE('',*,*,#13027,.T.);
#16546=ORIENTED_EDGE('',*,*,#13028,.F.);
#16547=ORIENTED_EDGE('',*,*,#13027,.F.);
#16548=ORIENTED_EDGE('',*,*,#13029,.T.);
#16549=ORIENTED_EDGE('',*,*,#13030,.T.);
#16550=ORIENTED_EDGE('',*,*,#13031,.T.);
#16551=ORIENTED_EDGE('',*,*,#13032,.T.);
#16552=ORIENTED_EDGE('',*,*,#13030,.F.);
#16553=ORIENTED_EDGE('',*,*,#13031,.F.);
#16554=ORIENTED_EDGE('',*,*,#13032,.F.);
#16555=ORIENTED_EDGE('',*,*,#13033,.T.);
#16556=ORIENTED_EDGE('',*,*,#13034,.F.);
#16557=ORIENTED_EDGE('',*,*,#13033,.F.);
#16558=ORIENTED_EDGE('',*,*,#13035,.F.);
#16559=ORIENTED_EDGE('',*,*,#13029,.F.);
#16560=ORIENTED_EDGE('',*,*,#13036,.T.);
#16561=ORIENTED_EDGE('',*,*,#13037,.T.);
#16562=ORIENTED_EDGE('',*,*,#13034,.T.);
#16563=ORIENTED_EDGE('',*,*,#13037,.F.);
#16564=ORIENTED_EDGE('',*,*,#13038,.F.);
#16565=ORIENTED_EDGE('',*,*,#13039,.F.);
#16566=ORIENTED_EDGE('',*,*,#13040,.F.);
#16567=ORIENTED_EDGE('',*,*,#13041,.F.);
#16568=ORIENTED_EDGE('',*,*,#13036,.F.);
#16569=ORIENTED_EDGE('',*,*,#13042,.T.);
#16570=ORIENTED_EDGE('',*,*,#13043,.F.);
#16571=ORIENTED_EDGE('',*,*,#13044,.T.);
#16572=ORIENTED_EDGE('',*,*,#13045,.T.);
#16573=ORIENTED_EDGE('',*,*,#13043,.T.);
#16574=ORIENTED_EDGE('',*,*,#13046,.T.);
#16575=ORIENTED_EDGE('',*,*,#13047,.T.);
#16576=ORIENTED_EDGE('',*,*,#13048,.T.);
#16577=ORIENTED_EDGE('',*,*,#13049,.T.);
#16578=ORIENTED_EDGE('',*,*,#13050,.T.);
#16579=ORIENTED_EDGE('',*,*,#13047,.F.);
#16580=ORIENTED_EDGE('',*,*,#13051,.T.);
#16581=ORIENTED_EDGE('',*,*,#13052,.F.);
#16582=ORIENTED_EDGE('',*,*,#13053,.F.);
#16583=ORIENTED_EDGE('',*,*,#13054,.F.);
#16584=ORIENTED_EDGE('',*,*,#13055,.F.);
#16585=ORIENTED_EDGE('',*,*,#13056,.F.);
#16586=ORIENTED_EDGE('',*,*,#13057,.F.);
#16587=ORIENTED_EDGE('',*,*,#13058,.F.);
#16588=ORIENTED_EDGE('',*,*,#13059,.F.);
#16589=ORIENTED_EDGE('',*,*,#13060,.F.);
#16590=ORIENTED_EDGE('',*,*,#13061,.F.);
#16591=ORIENTED_EDGE('',*,*,#13062,.F.);
#16592=ORIENTED_EDGE('',*,*,#13045,.F.);
#16593=ORIENTED_EDGE('',*,*,#13063,.F.);
#16594=ORIENTED_EDGE('',*,*,#13064,.F.);
#16595=ORIENTED_EDGE('',*,*,#13065,.F.);
#16596=ORIENTED_EDGE('',*,*,#13066,.F.);
#16597=ORIENTED_EDGE('',*,*,#13067,.F.);
#16598=ORIENTED_EDGE('',*,*,#13068,.F.);
#16599=ORIENTED_EDGE('',*,*,#13069,.F.);
#16600=ORIENTED_EDGE('',*,*,#13070,.F.);
#16601=ORIENTED_EDGE('',*,*,#13071,.F.);
#16602=ORIENTED_EDGE('',*,*,#13072,.F.);
#16603=ORIENTED_EDGE('',*,*,#13073,.F.);
#16604=ORIENTED_EDGE('',*,*,#13074,.F.);
#16605=ORIENTED_EDGE('',*,*,#13075,.F.);
#16606=ORIENTED_EDGE('',*,*,#13076,.F.);
#16607=ORIENTED_EDGE('',*,*,#13077,.F.);
#16608=ORIENTED_EDGE('',*,*,#13078,.F.);
#16609=ORIENTED_EDGE('',*,*,#13079,.F.);
#16610=ORIENTED_EDGE('',*,*,#13080,.F.);
#16611=ORIENTED_EDGE('',*,*,#13081,.F.);
#16612=ORIENTED_EDGE('',*,*,#13082,.F.);
#16613=ORIENTED_EDGE('',*,*,#13083,.F.);
#16614=ORIENTED_EDGE('',*,*,#13084,.F.);
#16615=ORIENTED_EDGE('',*,*,#13085,.F.);
#16616=ORIENTED_EDGE('',*,*,#13086,.F.);
#16617=ORIENTED_EDGE('',*,*,#13087,.F.);
#16618=ORIENTED_EDGE('',*,*,#13088,.F.);
#16619=ORIENTED_EDGE('',*,*,#13089,.F.);
#16620=ORIENTED_EDGE('',*,*,#13090,.F.);
#16621=ORIENTED_EDGE('',*,*,#13091,.F.);
#16622=ORIENTED_EDGE('',*,*,#13092,.T.);
#16623=ORIENTED_EDGE('',*,*,#13093,.T.);
#16624=ORIENTED_EDGE('',*,*,#13094,.F.);
#16625=ORIENTED_EDGE('',*,*,#13095,.T.);
#16626=ORIENTED_EDGE('',*,*,#13096,.F.);
#16627=ORIENTED_EDGE('',*,*,#13097,.F.);
#16628=ORIENTED_EDGE('',*,*,#13098,.F.);
#16629=ORIENTED_EDGE('',*,*,#13099,.F.);
#16630=ORIENTED_EDGE('',*,*,#13100,.F.);
#16631=ORIENTED_EDGE('',*,*,#13101,.F.);
#16632=ORIENTED_EDGE('',*,*,#13044,.F.);
#16633=ORIENTED_EDGE('',*,*,#13048,.F.);
#16634=ORIENTED_EDGE('',*,*,#13102,.T.);
#16635=ORIENTED_EDGE('',*,*,#13103,.F.);
#16636=ORIENTED_EDGE('',*,*,#13104,.F.);
#16637=ORIENTED_EDGE('',*,*,#13063,.T.);
#16638=ORIENTED_EDGE('',*,*,#13050,.F.);
#16639=ORIENTED_EDGE('',*,*,#13105,.F.);
#16640=ORIENTED_EDGE('',*,*,#13106,.F.);
#16641=ORIENTED_EDGE('',*,*,#13102,.F.);
#16642=ORIENTED_EDGE('',*,*,#13104,.T.);
#16643=ORIENTED_EDGE('',*,*,#13107,.F.);
#16644=ORIENTED_EDGE('',*,*,#13108,.T.);
#16645=ORIENTED_EDGE('',*,*,#13064,.T.);
#16646=ORIENTED_EDGE('',*,*,#13107,.T.);
#16647=ORIENTED_EDGE('',*,*,#13103,.T.);
#16648=ORIENTED_EDGE('',*,*,#13109,.T.);
#16649=ORIENTED_EDGE('',*,*,#13110,.T.);
#16650=ORIENTED_EDGE('',*,*,#13111,.T.);
#16651=ORIENTED_EDGE('',*,*,#13112,.T.);
#16652=ORIENTED_EDGE('',*,*,#13109,.F.);
#16653=ORIENTED_EDGE('',*,*,#13106,.T.);
#16654=ORIENTED_EDGE('',*,*,#13108,.F.);
#16655=ORIENTED_EDGE('',*,*,#13110,.F.);
#16656=ORIENTED_EDGE('',*,*,#13113,.T.);
#16657=ORIENTED_EDGE('',*,*,#13114,.F.);
#16658=ORIENTED_EDGE('',*,*,#13065,.T.);
#16659=ORIENTED_EDGE('',*,*,#13112,.F.);
#16660=ORIENTED_EDGE('',*,*,#13115,.F.);
#16661=ORIENTED_EDGE('',*,*,#13116,.F.);
#16662=ORIENTED_EDGE('',*,*,#13113,.F.);
#16663=ORIENTED_EDGE('',*,*,#13026,.T.);
#16664=ORIENTED_EDGE('',*,*,#13117,.T.);
#16665=ORIENTED_EDGE('',*,*,#13118,.T.);
#16666=ORIENTED_EDGE('',*,*,#13117,.F.);
#16667=ORIENTED_EDGE('',*,*,#13119,.F.);
#16668=ORIENTED_EDGE('',*,*,#13120,.T.);
#16669=ORIENTED_EDGE('',*,*,#13118,.F.);
#16670=ORIENTED_EDGE('',*,*,#13120,.F.);
#16671=ORIENTED_EDGE('',*,*,#13020,.T.);
#16672=ORIENTED_EDGE('',*,*,#13121,.T.);
#16673=ORIENTED_EDGE('',*,*,#13122,.T.);
#16674=ORIENTED_EDGE('',*,*,#13121,.F.);
#16675=ORIENTED_EDGE('',*,*,#13123,.F.);
#16676=ORIENTED_EDGE('',*,*,#13124,.T.);
#16677=ORIENTED_EDGE('',*,*,#13122,.F.);
#16678=ORIENTED_EDGE('',*,*,#13124,.F.);
#16679=ORIENTED_EDGE('',*,*,#13125,.T.);
#16680=ORIENTED_EDGE('',*,*,#13126,.T.);
#16681=ORIENTED_EDGE('',*,*,#13127,.T.);
#16682=ORIENTED_EDGE('',*,*,#13128,.T.);
#16683=ORIENTED_EDGE('',*,*,#13129,.F.);
#16684=ORIENTED_EDGE('',*,*,#13130,.T.);
#16685=ORIENTED_EDGE('',*,*,#13131,.T.);
#16686=ORIENTED_EDGE('',*,*,#13132,.F.);
#16687=ORIENTED_EDGE('',*,*,#13126,.F.);
#16688=ORIENTED_EDGE('',*,*,#13133,.F.);
#16689=ORIENTED_EDGE('',*,*,#13134,.F.);
#16690=ORIENTED_EDGE('',*,*,#13135,.F.);
#16691=ORIENTED_EDGE('',*,*,#13136,.T.);
#16692=ORIENTED_EDGE('',*,*,#13130,.F.);
#16693=ORIENTED_EDGE('',*,*,#13137,.T.);
#16694=ORIENTED_EDGE('',*,*,#13138,.T.);
#16695=ORIENTED_EDGE('',*,*,#13139,.T.);
#16696=ORIENTED_EDGE('',*,*,#13140,.T.);
#16697=ORIENTED_EDGE('',*,*,#13141,.F.);
#16698=ORIENTED_EDGE('',*,*,#13142,.T.);
#16699=ORIENTED_EDGE('',*,*,#13143,.F.);
#16700=ORIENTED_EDGE('',*,*,#13138,.F.);
#16701=ORIENTED_EDGE('',*,*,#13144,.F.);
#16702=ORIENTED_EDGE('',*,*,#13145,.T.);
#16703=ORIENTED_EDGE('',*,*,#13146,.F.);
#16704=ORIENTED_EDGE('',*,*,#13147,.F.);
#16705=ORIENTED_EDGE('',*,*,#13148,.F.);
#16706=ORIENTED_EDGE('',*,*,#13142,.F.);
#16707=ORIENTED_EDGE('',*,*,#13149,.T.);
#16708=ORIENTED_EDGE('',*,*,#13147,.T.);
#16709=ORIENTED_EDGE('',*,*,#13150,.T.);
#16710=ORIENTED_EDGE('',*,*,#13151,.T.);
#16711=ORIENTED_EDGE('',*,*,#13152,.T.);
#16712=ORIENTED_EDGE('',*,*,#13134,.T.);
#16713=ORIENTED_EDGE('',*,*,#13153,.T.);
#16714=ORIENTED_EDGE('',*,*,#13154,.T.);
#16715=ORIENTED_EDGE('',*,*,#13155,.T.);
#16716=ORIENTED_EDGE('',*,*,#13156,.T.);
#16717=ORIENTED_EDGE('',*,*,#13123,.T.);
#16718=ORIENTED_EDGE('',*,*,#13156,.F.);
#16719=ORIENTED_EDGE('',*,*,#13157,.F.);
#16720=ORIENTED_EDGE('',*,*,#13158,.F.);
#16721=ORIENTED_EDGE('',*,*,#13159,.F.);
#16722=ORIENTED_EDGE('',*,*,#13160,.F.);
#16723=ORIENTED_EDGE('',*,*,#13161,.F.);
#16724=ORIENTED_EDGE('',*,*,#13162,.F.);
#16725=ORIENTED_EDGE('',*,*,#13163,.F.);
#16726=ORIENTED_EDGE('',*,*,#13164,.F.);
#16727=ORIENTED_EDGE('',*,*,#13165,.F.);
#16728=ORIENTED_EDGE('',*,*,#13166,.F.);
#16729=ORIENTED_EDGE('',*,*,#13167,.F.);
#16730=ORIENTED_EDGE('',*,*,#13168,.F.);
#16731=ORIENTED_EDGE('',*,*,#13169,.F.);
#16732=ORIENTED_EDGE('',*,*,#13170,.F.);
#16733=ORIENTED_EDGE('',*,*,#13171,.F.);
#16734=ORIENTED_EDGE('',*,*,#13172,.T.);
#16735=ORIENTED_EDGE('',*,*,#13173,.T.);
#16736=ORIENTED_EDGE('',*,*,#13174,.F.);
#16737=ORIENTED_EDGE('',*,*,#13175,.F.);
#16738=ORIENTED_EDGE('',*,*,#13155,.F.);
#16739=ORIENTED_EDGE('',*,*,#13165,.T.);
#16740=ORIENTED_EDGE('',*,*,#13176,.T.);
#16741=ORIENTED_EDGE('',*,*,#13141,.T.);
#16742=ORIENTED_EDGE('',*,*,#13176,.F.);
#16743=ORIENTED_EDGE('',*,*,#13175,.T.);
#16744=ORIENTED_EDGE('',*,*,#13177,.T.);
#16745=ORIENTED_EDGE('',*,*,#13129,.T.);
#16746=ORIENTED_EDGE('',*,*,#13177,.F.);
#16747=ORIENTED_EDGE('',*,*,#13166,.T.);
#16748=ORIENTED_EDGE('',*,*,#13178,.T.);
#16749=ORIENTED_EDGE('',*,*,#13119,.T.);
#16750=ORIENTED_EDGE('',*,*,#13178,.F.);
#16751=ORIENTED_EDGE('',*,*,#13174,.T.);
#16752=ORIENTED_EDGE('',*,*,#13179,.T.);
#16753=ORIENTED_EDGE('',*,*,#13180,.T.);
#16754=ORIENTED_EDGE('',*,*,#13179,.F.);
#16755=ORIENTED_EDGE('',*,*,#13181,.F.);
#16756=ORIENTED_EDGE('',*,*,#13182,.T.);
#16757=ORIENTED_EDGE('',*,*,#13180,.F.);
#16758=ORIENTED_EDGE('',*,*,#13182,.F.);
#16759=ORIENTED_EDGE('',*,*,#13167,.T.);
#16760=ORIENTED_EDGE('',*,*,#13183,.T.);
#16761=ORIENTED_EDGE('',*,*,#13184,.T.);
#16762=ORIENTED_EDGE('',*,*,#13183,.F.);
#16763=ORIENTED_EDGE('',*,*,#13185,.F.);
#16764=ORIENTED_EDGE('',*,*,#13186,.T.);
#16765=ORIENTED_EDGE('',*,*,#13184,.F.);
#16766=ORIENTED_EDGE('',*,*,#13186,.F.);
#16767=ORIENTED_EDGE('',*,*,#13187,.T.);
#16768=ORIENTED_EDGE('',*,*,#13188,.F.);
#16769=ORIENTED_EDGE('',*,*,#13189,.T.);
#16770=ORIENTED_EDGE('',*,*,#13080,.T.);
#16771=ORIENTED_EDGE('',*,*,#13188,.T.);
#16772=ORIENTED_EDGE('',*,*,#13190,.T.);
#16773=ORIENTED_EDGE('',*,*,#13191,.T.);
#16774=ORIENTED_EDGE('',*,*,#13192,.T.);
#16775=ORIENTED_EDGE('',*,*,#13193,.T.);
#16776=ORIENTED_EDGE('',*,*,#13194,.T.);
#16777=ORIENTED_EDGE('',*,*,#13191,.F.);
#16778=ORIENTED_EDGE('',*,*,#13195,.T.);
#16779=ORIENTED_EDGE('',*,*,#13189,.F.);
#16780=ORIENTED_EDGE('',*,*,#13192,.F.);
#16781=ORIENTED_EDGE('',*,*,#13196,.T.);
#16782=ORIENTED_EDGE('',*,*,#13197,.F.);
#16783=ORIENTED_EDGE('',*,*,#13198,.F.);
#16784=ORIENTED_EDGE('',*,*,#13081,.T.);
#16785=ORIENTED_EDGE('',*,*,#13194,.F.);
#16786=ORIENTED_EDGE('',*,*,#13199,.F.);
#16787=ORIENTED_EDGE('',*,*,#13200,.F.);
#16788=ORIENTED_EDGE('',*,*,#13196,.F.);
#16789=ORIENTED_EDGE('',*,*,#13198,.T.);
#16790=ORIENTED_EDGE('',*,*,#13201,.F.);
#16791=ORIENTED_EDGE('',*,*,#13202,.T.);
#16792=ORIENTED_EDGE('',*,*,#13082,.T.);
#16793=ORIENTED_EDGE('',*,*,#13201,.T.);
#16794=ORIENTED_EDGE('',*,*,#13197,.T.);
#16795=ORIENTED_EDGE('',*,*,#13203,.T.);
#16796=ORIENTED_EDGE('',*,*,#13204,.T.);
#16797=ORIENTED_EDGE('',*,*,#13205,.T.);
#16798=ORIENTED_EDGE('',*,*,#13206,.T.);
#16799=ORIENTED_EDGE('',*,*,#13203,.F.);
#16800=ORIENTED_EDGE('',*,*,#13200,.T.);
#16801=ORIENTED_EDGE('',*,*,#13202,.F.);
#16802=ORIENTED_EDGE('',*,*,#13204,.F.);
#16803=ORIENTED_EDGE('',*,*,#13207,.T.);
#16804=ORIENTED_EDGE('',*,*,#13208,.F.);
#16805=ORIENTED_EDGE('',*,*,#13083,.T.);
#16806=ORIENTED_EDGE('',*,*,#13206,.F.);
#16807=ORIENTED_EDGE('',*,*,#13209,.F.);
#16808=ORIENTED_EDGE('',*,*,#13210,.F.);
#16809=ORIENTED_EDGE('',*,*,#13207,.F.);
#16810=ORIENTED_EDGE('',*,*,#13101,.T.);
#16811=ORIENTED_EDGE('',*,*,#13211,.T.);
#16812=ORIENTED_EDGE('',*,*,#13185,.T.);
#16813=ORIENTED_EDGE('',*,*,#13211,.F.);
#16814=ORIENTED_EDGE('',*,*,#13062,.T.);
#16815=ORIENTED_EDGE('',*,*,#13212,.T.);
#16816=ORIENTED_EDGE('',*,*,#13181,.T.);
#16817=ORIENTED_EDGE('',*,*,#13212,.F.);
#16818=ORIENTED_EDGE('',*,*,#13213,.T.);
#16819=ORIENTED_EDGE('',*,*,#13214,.T.);
#16820=ORIENTED_EDGE('',*,*,#13215,.T.);
#16821=ORIENTED_EDGE('',*,*,#13216,.T.);
#16822=ORIENTED_EDGE('',*,*,#13217,.T.);
#16823=ORIENTED_EDGE('',*,*,#13218,.T.);
#16824=ORIENTED_EDGE('',*,*,#13215,.F.);
#16825=ORIENTED_EDGE('',*,*,#13219,.T.);
#16826=ORIENTED_EDGE('',*,*,#13220,.T.);
#16827=ORIENTED_EDGE('',*,*,#13068,.T.);
#16828=ORIENTED_EDGE('',*,*,#13217,.F.);
#16829=ORIENTED_EDGE('',*,*,#13221,.T.);
#16830=ORIENTED_EDGE('',*,*,#13222,.T.);
#16831=ORIENTED_EDGE('',*,*,#13223,.T.);
#16832=ORIENTED_EDGE('',*,*,#13220,.F.);
#16833=ORIENTED_EDGE('',*,*,#13224,.T.);
#16834=ORIENTED_EDGE('',*,*,#13225,.T.);
#16835=ORIENTED_EDGE('',*,*,#13226,.T.);
#16836=ORIENTED_EDGE('',*,*,#13222,.F.);
#16837=ORIENTED_EDGE('',*,*,#13227,.T.);
#16838=ORIENTED_EDGE('',*,*,#13227,.F.);
#16839=ORIENTED_EDGE('',*,*,#13224,.F.);
#16840=ORIENTED_EDGE('',*,*,#13221,.F.);
#16841=ORIENTED_EDGE('',*,*,#13219,.F.);
#16842=ORIENTED_EDGE('',*,*,#13214,.F.);
#16843=ORIENTED_EDGE('',*,*,#13228,.F.);
#16844=ORIENTED_EDGE('',*,*,#13229,.T.);
#16845=ORIENTED_EDGE('',*,*,#13230,.T.);
#16846=ORIENTED_EDGE('',*,*,#13231,.T.);
#16847=ORIENTED_EDGE('',*,*,#13232,.T.);
#16848=ORIENTED_EDGE('',*,*,#13230,.F.);
#16849=ORIENTED_EDGE('',*,*,#13233,.F.);
#16850=ORIENTED_EDGE('',*,*,#13234,.F.);
#16851=ORIENTED_EDGE('',*,*,#13235,.F.);
#16852=ORIENTED_EDGE('',*,*,#13099,.T.);
#16853=ORIENTED_EDGE('',*,*,#13236,.T.);
#16854=ORIENTED_EDGE('',*,*,#13237,.T.);
#16855=ORIENTED_EDGE('',*,*,#13238,.F.);
#16856=ORIENTED_EDGE('',*,*,#13098,.T.);
#16857=ORIENTED_EDGE('',*,*,#13239,.T.);
#16858=ORIENTED_EDGE('',*,*,#13240,.T.);
#16859=ORIENTED_EDGE('',*,*,#13236,.F.);
#16860=ORIENTED_EDGE('',*,*,#13241,.T.);
#16861=ORIENTED_EDGE('',*,*,#13242,.T.);
#16862=ORIENTED_EDGE('',*,*,#13243,.T.);
#16863=ORIENTED_EDGE('',*,*,#13096,.T.);
#16864=ORIENTED_EDGE('',*,*,#13097,.T.);
#16865=ORIENTED_EDGE('',*,*,#13243,.F.);
#16866=ORIENTED_EDGE('',*,*,#13244,.T.);
#16867=ORIENTED_EDGE('',*,*,#13239,.F.);
#16868=ORIENTED_EDGE('',*,*,#13245,.T.);
#16869=ORIENTED_EDGE('',*,*,#13241,.F.);
#16870=ORIENTED_EDGE('',*,*,#13100,.T.);
#16871=ORIENTED_EDGE('',*,*,#13238,.T.);
#16872=ORIENTED_EDGE('',*,*,#13240,.F.);
#16873=ORIENTED_EDGE('',*,*,#13246,.F.);
#16874=ORIENTED_EDGE('',*,*,#13247,.F.);
#16875=ORIENTED_EDGE('',*,*,#13248,.T.);
#16876=ORIENTED_EDGE('',*,*,#13244,.F.);
#16877=ORIENTED_EDGE('',*,*,#13249,.T.);
#16878=ORIENTED_EDGE('',*,*,#13250,.T.);
#16879=ORIENTED_EDGE('',*,*,#13246,.T.);
#16880=ORIENTED_EDGE('',*,*,#13242,.F.);
#16881=ORIENTED_EDGE('',*,*,#13251,.T.);
#16882=ORIENTED_EDGE('',*,*,#13252,.T.);
#16883=ORIENTED_EDGE('',*,*,#13249,.F.);
#16884=ORIENTED_EDGE('',*,*,#13089,.T.);
#16885=ORIENTED_EDGE('',*,*,#13253,.T.);
#16886=ORIENTED_EDGE('',*,*,#13254,.T.);
#16887=ORIENTED_EDGE('',*,*,#13255,.F.);
#16888=ORIENTED_EDGE('',*,*,#13088,.T.);
#16889=ORIENTED_EDGE('',*,*,#13256,.T.);
#16890=ORIENTED_EDGE('',*,*,#13257,.T.);
#16891=ORIENTED_EDGE('',*,*,#13253,.F.);
#16892=ORIENTED_EDGE('',*,*,#13258,.T.);
#16893=ORIENTED_EDGE('',*,*,#13259,.T.);
#16894=ORIENTED_EDGE('',*,*,#13260,.T.);
#16895=ORIENTED_EDGE('',*,*,#13086,.T.);
#16896=ORIENTED_EDGE('',*,*,#13087,.T.);
#16897=ORIENTED_EDGE('',*,*,#13260,.F.);
#16898=ORIENTED_EDGE('',*,*,#13261,.T.);
#16899=ORIENTED_EDGE('',*,*,#13256,.F.);
#16900=ORIENTED_EDGE('',*,*,#13262,.T.);
#16901=ORIENTED_EDGE('',*,*,#13258,.F.);
#16902=ORIENTED_EDGE('',*,*,#13090,.T.);
#16903=ORIENTED_EDGE('',*,*,#13255,.T.);
#16904=ORIENTED_EDGE('',*,*,#13257,.F.);
#16905=ORIENTED_EDGE('',*,*,#13263,.F.);
#16906=ORIENTED_EDGE('',*,*,#13264,.F.);
#16907=ORIENTED_EDGE('',*,*,#13265,.T.);
#16908=ORIENTED_EDGE('',*,*,#13261,.F.);
#16909=ORIENTED_EDGE('',*,*,#13266,.T.);
#16910=ORIENTED_EDGE('',*,*,#13267,.T.);
#16911=ORIENTED_EDGE('',*,*,#13263,.T.);
#16912=ORIENTED_EDGE('',*,*,#13259,.F.);
#16913=ORIENTED_EDGE('',*,*,#13268,.T.);
#16914=ORIENTED_EDGE('',*,*,#13269,.T.);
#16915=ORIENTED_EDGE('',*,*,#13266,.F.);
#16916=ORIENTED_EDGE('',*,*,#13270,.T.);
#16917=ORIENTED_EDGE('',*,*,#13234,.T.);
#16918=ORIENTED_EDGE('',*,*,#13271,.T.);
#16919=ORIENTED_EDGE('',*,*,#13061,.T.);
#16920=ORIENTED_EDGE('',*,*,#13114,.T.);
#16921=ORIENTED_EDGE('',*,*,#13272,.T.);
#16922=ORIENTED_EDGE('',*,*,#13273,.T.);
#16923=ORIENTED_EDGE('',*,*,#13066,.T.);
#16924=ORIENTED_EDGE('',*,*,#13272,.F.);
#16925=ORIENTED_EDGE('',*,*,#13116,.T.);
#16926=ORIENTED_EDGE('',*,*,#13274,.F.);
#16927=ORIENTED_EDGE('',*,*,#13275,.T.);
#16928=ORIENTED_EDGE('',*,*,#13276,.T.);
#16929=ORIENTED_EDGE('',*,*,#13277,.T.);
#16930=ORIENTED_EDGE('',*,*,#13278,.T.);
#16931=ORIENTED_EDGE('',*,*,#13077,.T.);
#16932=ORIENTED_EDGE('',*,*,#13277,.F.);
#16933=ORIENTED_EDGE('',*,*,#13279,.F.);
#16934=ORIENTED_EDGE('',*,*,#13280,.F.);
#16935=ORIENTED_EDGE('',*,*,#13281,.T.);
#16936=ORIENTED_EDGE('',*,*,#13282,.T.);
#16937=ORIENTED_EDGE('',*,*,#13283,.T.);
#16938=ORIENTED_EDGE('',*,*,#13072,.T.);
#16939=ORIENTED_EDGE('',*,*,#13284,.T.);
#16940=ORIENTED_EDGE('',*,*,#13071,.T.);
#16941=ORIENTED_EDGE('',*,*,#13285,.T.);
#16942=ORIENTED_EDGE('',*,*,#13286,.T.);
#16943=ORIENTED_EDGE('',*,*,#13284,.F.);
#16944=ORIENTED_EDGE('',*,*,#13070,.T.);
#16945=ORIENTED_EDGE('',*,*,#13287,.T.);
#16946=ORIENTED_EDGE('',*,*,#13288,.T.);
#16947=ORIENTED_EDGE('',*,*,#13285,.F.);
#16948=ORIENTED_EDGE('',*,*,#13289,.T.);
#16949=ORIENTED_EDGE('',*,*,#13073,.T.);
#16950=ORIENTED_EDGE('',*,*,#13283,.F.);
#16951=ORIENTED_EDGE('',*,*,#13290,.T.);
#16952=ORIENTED_EDGE('',*,*,#13291,.T.);
#16953=ORIENTED_EDGE('',*,*,#13074,.T.);
#16954=ORIENTED_EDGE('',*,*,#13289,.F.);
#16955=ORIENTED_EDGE('',*,*,#13292,.T.);
#16956=ORIENTED_EDGE('',*,*,#13293,.T.);
#16957=ORIENTED_EDGE('',*,*,#13075,.T.);
#16958=ORIENTED_EDGE('',*,*,#13291,.F.);
#16959=ORIENTED_EDGE('',*,*,#13294,.T.);
#16960=ORIENTED_EDGE('',*,*,#13076,.T.);
#16961=ORIENTED_EDGE('',*,*,#13293,.F.);
#16962=ORIENTED_EDGE('',*,*,#13295,.T.);
#16963=ORIENTED_EDGE('',*,*,#13276,.F.);
#16964=ORIENTED_EDGE('',*,*,#13295,.F.);
#16965=ORIENTED_EDGE('',*,*,#13296,.T.);
#16966=ORIENTED_EDGE('',*,*,#13297,.T.);
#16967=ORIENTED_EDGE('',*,*,#13279,.T.);
#16968=ORIENTED_EDGE('',*,*,#13294,.F.);
#16969=ORIENTED_EDGE('',*,*,#13298,.T.);
#16970=ORIENTED_EDGE('',*,*,#13299,.T.);
#16971=ORIENTED_EDGE('',*,*,#13296,.F.);
#16972=ORIENTED_EDGE('',*,*,#13292,.F.);
#16973=ORIENTED_EDGE('',*,*,#13300,.T.);
#16974=ORIENTED_EDGE('',*,*,#13301,.T.);
#16975=ORIENTED_EDGE('',*,*,#13298,.F.);
#16976=ORIENTED_EDGE('',*,*,#13290,.F.);
#16977=ORIENTED_EDGE('',*,*,#13302,.T.);
#16978=ORIENTED_EDGE('',*,*,#13303,.T.);
#16979=ORIENTED_EDGE('',*,*,#13300,.F.);
#16980=ORIENTED_EDGE('',*,*,#13282,.F.);
#16981=ORIENTED_EDGE('',*,*,#13304,.T.);
#16982=ORIENTED_EDGE('',*,*,#13305,.T.);
#16983=ORIENTED_EDGE('',*,*,#13302,.F.);
#16984=ORIENTED_EDGE('',*,*,#13286,.F.);
#16985=ORIENTED_EDGE('',*,*,#13306,.F.);
#16986=ORIENTED_EDGE('',*,*,#13307,.F.);
#16987=ORIENTED_EDGE('',*,*,#13304,.F.);
#16988=ORIENTED_EDGE('',*,*,#13288,.F.);
#16989=ORIENTED_EDGE('',*,*,#13308,.T.);
#16990=ORIENTED_EDGE('',*,*,#13309,.F.);
#16991=ORIENTED_EDGE('',*,*,#13306,.T.);
#16992=ORIENTED_EDGE('',*,*,#13310,.T.);
#16993=ORIENTED_EDGE('',*,*,#13311,.T.);
#16994=ORIENTED_EDGE('',*,*,#13312,.T.);
#16995=ORIENTED_EDGE('',*,*,#13054,.T.);
#16996=ORIENTED_EDGE('',*,*,#13313,.T.);
#16997=ORIENTED_EDGE('',*,*,#13055,.T.);
#16998=ORIENTED_EDGE('',*,*,#13312,.F.);
#16999=ORIENTED_EDGE('',*,*,#13314,.T.);
#17000=ORIENTED_EDGE('',*,*,#13315,.T.);
#17001=ORIENTED_EDGE('',*,*,#13056,.T.);
#17002=ORIENTED_EDGE('',*,*,#13313,.F.);
#17003=ORIENTED_EDGE('',*,*,#13316,.T.);
#17004=ORIENTED_EDGE('',*,*,#13317,.T.);
#17005=ORIENTED_EDGE('',*,*,#13057,.T.);
#17006=ORIENTED_EDGE('',*,*,#13315,.F.);
#17007=ORIENTED_EDGE('',*,*,#13318,.T.);
#17008=ORIENTED_EDGE('',*,*,#13319,.T.);
#17009=ORIENTED_EDGE('',*,*,#13058,.T.);
#17010=ORIENTED_EDGE('',*,*,#13317,.F.);
#17011=ORIENTED_EDGE('',*,*,#13320,.T.);
#17012=ORIENTED_EDGE('',*,*,#13321,.T.);
#17013=ORIENTED_EDGE('',*,*,#13059,.T.);
#17014=ORIENTED_EDGE('',*,*,#13319,.F.);
#17015=ORIENTED_EDGE('',*,*,#13322,.T.);
#17016=ORIENTED_EDGE('',*,*,#13060,.T.);
#17017=ORIENTED_EDGE('',*,*,#13321,.F.);
#17018=ORIENTED_EDGE('',*,*,#13323,.T.);
#17019=ORIENTED_EDGE('',*,*,#13270,.F.);
#17020=ORIENTED_EDGE('',*,*,#13324,.T.);
#17021=ORIENTED_EDGE('',*,*,#13325,.T.);
#17022=ORIENTED_EDGE('',*,*,#13310,.F.);
#17023=ORIENTED_EDGE('',*,*,#13053,.T.);
#17024=ORIENTED_EDGE('',*,*,#13326,.T.);
#17025=ORIENTED_EDGE('',*,*,#13324,.F.);
#17026=ORIENTED_EDGE('',*,*,#13052,.T.);
#17027=ORIENTED_EDGE('',*,*,#13271,.F.);
#17028=ORIENTED_EDGE('',*,*,#13318,.F.);
#17029=ORIENTED_EDGE('',*,*,#13327,.T.);
#17030=ORIENTED_EDGE('',*,*,#13328,.F.);
#17031=ORIENTED_EDGE('',*,*,#13329,.F.);
#17032=ORIENTED_EDGE('',*,*,#13316,.F.);
#17033=ORIENTED_EDGE('',*,*,#13330,.T.);
#17034=ORIENTED_EDGE('',*,*,#13331,.F.);
#17035=ORIENTED_EDGE('',*,*,#13327,.F.);
#17036=ORIENTED_EDGE('',*,*,#13314,.F.);
#17037=ORIENTED_EDGE('',*,*,#13332,.T.);
#17038=ORIENTED_EDGE('',*,*,#13333,.F.);
#17039=ORIENTED_EDGE('',*,*,#13330,.F.);
#17040=ORIENTED_EDGE('',*,*,#13311,.F.);
#17041=ORIENTED_EDGE('',*,*,#13334,.T.);
#17042=ORIENTED_EDGE('',*,*,#13335,.F.);
#17043=ORIENTED_EDGE('',*,*,#13332,.F.);
#17044=ORIENTED_EDGE('',*,*,#13325,.F.);
#17045=ORIENTED_EDGE('',*,*,#13336,.T.);
#17046=ORIENTED_EDGE('',*,*,#13337,.F.);
#17047=ORIENTED_EDGE('',*,*,#13334,.F.);
#17048=ORIENTED_EDGE('',*,*,#13223,.F.);
#17049=ORIENTED_EDGE('',*,*,#13338,.T.);
#17050=ORIENTED_EDGE('',*,*,#13287,.F.);
#17051=ORIENTED_EDGE('',*,*,#13069,.T.);
#17052=ORIENTED_EDGE('',*,*,#13226,.F.);
#17053=ORIENTED_EDGE('',*,*,#13339,.F.);
#17054=ORIENTED_EDGE('',*,*,#13308,.F.);
#17055=ORIENTED_EDGE('',*,*,#13338,.F.);
#17056=ORIENTED_EDGE('',*,*,#13218,.F.);
#17057=ORIENTED_EDGE('',*,*,#13067,.T.);
#17058=ORIENTED_EDGE('',*,*,#13273,.F.);
#17059=ORIENTED_EDGE('',*,*,#13340,.T.);
#17060=ORIENTED_EDGE('',*,*,#13216,.F.);
#17061=ORIENTED_EDGE('',*,*,#13340,.F.);
#17062=ORIENTED_EDGE('',*,*,#13275,.F.);
#17063=ORIENTED_EDGE('',*,*,#13341,.F.);
#17064=ORIENTED_EDGE('',*,*,#13342,.T.);
#17065=ORIENTED_EDGE('',*,*,#13343,.T.);
#17066=ORIENTED_EDGE('',*,*,#13084,.T.);
#17067=ORIENTED_EDGE('',*,*,#13208,.T.);
#17068=ORIENTED_EDGE('',*,*,#13187,.F.);
#17069=ORIENTED_EDGE('',*,*,#13079,.T.);
#17070=ORIENTED_EDGE('',*,*,#13344,.T.);
#17071=ORIENTED_EDGE('',*,*,#13345,.T.);
#17072=ORIENTED_EDGE('',*,*,#13190,.F.);
#17073=ORIENTED_EDGE('',*,*,#13078,.T.);
#17074=ORIENTED_EDGE('',*,*,#13278,.F.);
#17075=ORIENTED_EDGE('',*,*,#13346,.T.);
#17076=ORIENTED_EDGE('',*,*,#13344,.F.);
#17077=ORIENTED_EDGE('',*,*,#13342,.F.);
#17078=ORIENTED_EDGE('',*,*,#13210,.T.);
#17079=ORIENTED_EDGE('',*,*,#13347,.F.);
#17080=ORIENTED_EDGE('',*,*,#13348,.T.);
#17081=ORIENTED_EDGE('',*,*,#13195,.F.);
#17082=ORIENTED_EDGE('',*,*,#13345,.F.);
#17083=ORIENTED_EDGE('',*,*,#13349,.F.);
#17084=ORIENTED_EDGE('',*,*,#13350,.F.);
#17085=ORIENTED_EDGE('',*,*,#13346,.F.);
#17086=ORIENTED_EDGE('',*,*,#13281,.F.);
#17087=ORIENTED_EDGE('',*,*,#13351,.F.);
#17088=ORIENTED_EDGE('',*,*,#13349,.T.);
#17089=ORIENTED_EDGE('',*,*,#13352,.T.);
#17090=ORIENTED_EDGE('',*,*,#13328,.T.);
#17091=ORIENTED_EDGE('',*,*,#13353,.T.);
#17092=ORIENTED_EDGE('',*,*,#13157,.T.);
#17093=ORIENTED_EDGE('',*,*,#13354,.T.);
#17094=ORIENTED_EDGE('',*,*,#13158,.T.);
#17095=ORIENTED_EDGE('',*,*,#13353,.F.);
#17096=ORIENTED_EDGE('',*,*,#13331,.T.);
#17097=ORIENTED_EDGE('',*,*,#13355,.T.);
#17098=ORIENTED_EDGE('',*,*,#13159,.T.);
#17099=ORIENTED_EDGE('',*,*,#13354,.F.);
#17100=ORIENTED_EDGE('',*,*,#13333,.T.);
#17101=ORIENTED_EDGE('',*,*,#13356,.T.);
#17102=ORIENTED_EDGE('',*,*,#13160,.T.);
#17103=ORIENTED_EDGE('',*,*,#13355,.F.);
#17104=ORIENTED_EDGE('',*,*,#13335,.T.);
#17105=ORIENTED_EDGE('',*,*,#13357,.T.);
#17106=ORIENTED_EDGE('',*,*,#13161,.T.);
#17107=ORIENTED_EDGE('',*,*,#13356,.F.);
#17108=ORIENTED_EDGE('',*,*,#13337,.T.);
#17109=ORIENTED_EDGE('',*,*,#13358,.T.);
#17110=ORIENTED_EDGE('',*,*,#13162,.T.);
#17111=ORIENTED_EDGE('',*,*,#13357,.F.);
#17112=ORIENTED_EDGE('',*,*,#13359,.T.);
#17113=ORIENTED_EDGE('',*,*,#13360,.T.);
#17114=ORIENTED_EDGE('',*,*,#13163,.T.);
#17115=ORIENTED_EDGE('',*,*,#13358,.F.);
#17116=ORIENTED_EDGE('',*,*,#13361,.T.);
#17117=ORIENTED_EDGE('',*,*,#13352,.F.);
#17118=ORIENTED_EDGE('',*,*,#13164,.T.);
#17119=ORIENTED_EDGE('',*,*,#13360,.F.);
#17120=ORIENTED_EDGE('',*,*,#13362,.T.);
#17121=ORIENTED_EDGE('',*,*,#13363,.T.);
#17122=ORIENTED_EDGE('',*,*,#13364,.T.);
#17123=ORIENTED_EDGE('',*,*,#13365,.T.);
#17124=ORIENTED_EDGE('',*,*,#13364,.F.);
#17125=ORIENTED_EDGE('',*,*,#13366,.F.);
#17126=ORIENTED_EDGE('',*,*,#13154,.F.);
#17127=ORIENTED_EDGE('',*,*,#13367,.F.);
#17128=ORIENTED_EDGE('',*,*,#13095,.F.);
#17129=ORIENTED_EDGE('',*,*,#13368,.F.);
#17130=ORIENTED_EDGE('',*,*,#13151,.F.);
#17131=ORIENTED_EDGE('',*,*,#13369,.F.);
#17132=ORIENTED_EDGE('',*,*,#13140,.F.);
#17133=ORIENTED_EDGE('',*,*,#13370,.F.);
#17134=ORIENTED_EDGE('',*,*,#13093,.F.);
#17135=ORIENTED_EDGE('',*,*,#13371,.T.);
#17136=ORIENTED_EDGE('',*,*,#13363,.F.);
#17137=ORIENTED_EDGE('',*,*,#13371,.F.);
#17138=ORIENTED_EDGE('',*,*,#13092,.F.);
#17139=ORIENTED_EDGE('',*,*,#13372,.F.);
#17140=ORIENTED_EDGE('',*,*,#13128,.F.);
#17141=ORIENTED_EDGE('',*,*,#13365,.F.);
#17142=ORIENTED_EDGE('',*,*,#13373,.T.);
#17143=ORIENTED_EDGE('',*,*,#13042,.F.);
#17144=ORIENTED_EDGE('',*,*,#13085,.T.);
#17145=ORIENTED_EDGE('',*,*,#13343,.F.);
#17146=ORIENTED_EDGE('',*,*,#13374,.T.);
#17147=ORIENTED_EDGE('',*,*,#13046,.F.);
#17148=ORIENTED_EDGE('',*,*,#13051,.F.);
#17149=ORIENTED_EDGE('',*,*,#13374,.F.);
#17150=ORIENTED_EDGE('',*,*,#13348,.F.);
#17151=ORIENTED_EDGE('',*,*,#13375,.F.);
#17152=ORIENTED_EDGE('',*,*,#13367,.T.);
#17153=ORIENTED_EDGE('',*,*,#13153,.F.);
#17154=ORIENTED_EDGE('',*,*,#13133,.T.);
#17155=ORIENTED_EDGE('',*,*,#13125,.F.);
#17156=ORIENTED_EDGE('',*,*,#13372,.T.);
#17157=ORIENTED_EDGE('',*,*,#13091,.T.);
#17158=ORIENTED_EDGE('',*,*,#13132,.T.);
#17159=ORIENTED_EDGE('',*,*,#13376,.T.);
#17160=ORIENTED_EDGE('',*,*,#13135,.T.);
#17161=ORIENTED_EDGE('',*,*,#13152,.F.);
#17162=ORIENTED_EDGE('',*,*,#13366,.T.);
#17163=ORIENTED_EDGE('',*,*,#13127,.F.);
#17164=ORIENTED_EDGE('',*,*,#13376,.F.);
#17165=ORIENTED_EDGE('',*,*,#13131,.F.);
#17166=ORIENTED_EDGE('',*,*,#13136,.F.);
#17167=ORIENTED_EDGE('',*,*,#13370,.T.);
#17168=ORIENTED_EDGE('',*,*,#13139,.F.);
#17169=ORIENTED_EDGE('',*,*,#13143,.T.);
#17170=ORIENTED_EDGE('',*,*,#13148,.T.);
#17171=ORIENTED_EDGE('',*,*,#13149,.F.);
#17172=ORIENTED_EDGE('',*,*,#13368,.T.);
#17173=ORIENTED_EDGE('',*,*,#13094,.T.);
#17174=ORIENTED_EDGE('',*,*,#13146,.T.);
#17175=ORIENTED_EDGE('',*,*,#13377,.T.);
#17176=ORIENTED_EDGE('',*,*,#13144,.T.);
#17177=ORIENTED_EDGE('',*,*,#13137,.F.);
#17178=ORIENTED_EDGE('',*,*,#13369,.T.);
#17179=ORIENTED_EDGE('',*,*,#13150,.F.);
#17180=ORIENTED_EDGE('',*,*,#13377,.F.);
#17181=ORIENTED_EDGE('',*,*,#13145,.F.);
#17182=ORIENTED_EDGE('',*,*,#13378,.T.);
#17183=ORIENTED_EDGE('',*,*,#13379,.T.);
#17184=ORIENTED_EDGE('',*,*,#13380,.T.);
#17185=ORIENTED_EDGE('',*,*,#13168,.T.);
#17186=ORIENTED_EDGE('',*,*,#13381,.T.);
#17187=ORIENTED_EDGE('',*,*,#13169,.T.);
#17188=ORIENTED_EDGE('',*,*,#13380,.F.);
#17189=ORIENTED_EDGE('',*,*,#13382,.T.);
#17190=ORIENTED_EDGE('',*,*,#13383,.T.);
#17191=ORIENTED_EDGE('',*,*,#13170,.T.);
#17192=ORIENTED_EDGE('',*,*,#13381,.F.);
#17193=ORIENTED_EDGE('',*,*,#13384,.T.);
#17194=ORIENTED_EDGE('',*,*,#13378,.F.);
#17195=ORIENTED_EDGE('',*,*,#13171,.T.);
#17196=ORIENTED_EDGE('',*,*,#13383,.F.);
#17197=ORIENTED_EDGE('',*,*,#13385,.T.);
#17198=ORIENTED_EDGE('',*,*,#13382,.F.);
#17199=ORIENTED_EDGE('',*,*,#13386,.T.);
#17200=ORIENTED_EDGE('',*,*,#13387,.T.);
#17201=ORIENTED_EDGE('',*,*,#13388,.F.);
#17202=ORIENTED_EDGE('',*,*,#13379,.F.);
#17203=ORIENTED_EDGE('',*,*,#13389,.T.);
#17204=ORIENTED_EDGE('',*,*,#13390,.T.);
#17205=ORIENTED_EDGE('',*,*,#13386,.F.);
#17206=ORIENTED_EDGE('',*,*,#13391,.T.);
#17207=ORIENTED_EDGE('',*,*,#13392,.T.);
#17208=ORIENTED_EDGE('',*,*,#13393,.T.);
#17209=ORIENTED_EDGE('',*,*,#13038,.T.);
#17210=ORIENTED_EDGE('',*,*,#13394,.T.);
#17211=ORIENTED_EDGE('',*,*,#13039,.T.);
#17212=ORIENTED_EDGE('',*,*,#13393,.F.);
#17213=ORIENTED_EDGE('',*,*,#13395,.T.);
#17214=ORIENTED_EDGE('',*,*,#13396,.T.);
#17215=ORIENTED_EDGE('',*,*,#13040,.T.);
#17216=ORIENTED_EDGE('',*,*,#13394,.F.);
#17217=ORIENTED_EDGE('',*,*,#13397,.T.);
#17218=ORIENTED_EDGE('',*,*,#13391,.F.);
#17219=ORIENTED_EDGE('',*,*,#13041,.T.);
#17220=ORIENTED_EDGE('',*,*,#13396,.F.);
#17221=ORIENTED_EDGE('',*,*,#13398,.T.);
#17222=ORIENTED_EDGE('',*,*,#13395,.F.);
#17223=ORIENTED_EDGE('',*,*,#13399,.T.);
#17224=ORIENTED_EDGE('',*,*,#13400,.T.);
#17225=ORIENTED_EDGE('',*,*,#13401,.F.);
#17226=ORIENTED_EDGE('',*,*,#13392,.F.);
#17227=ORIENTED_EDGE('',*,*,#13402,.T.);
#17228=ORIENTED_EDGE('',*,*,#13403,.T.);
#17229=ORIENTED_EDGE('',*,*,#13399,.F.);
#17230=ORIENTED_EDGE('',*,*,#13398,.F.);
#17231=ORIENTED_EDGE('',*,*,#13404,.T.);
#17232=ORIENTED_EDGE('',*,*,#13405,.T.);
#17233=ORIENTED_EDGE('',*,*,#13402,.F.);
#17234=ORIENTED_EDGE('',*,*,#13397,.F.);
#17235=ORIENTED_EDGE('',*,*,#13401,.T.);
#17236=ORIENTED_EDGE('',*,*,#13406,.T.);
#17237=ORIENTED_EDGE('',*,*,#13404,.F.);
#17238=ORIENTED_EDGE('',*,*,#13385,.F.);
#17239=ORIENTED_EDGE('',*,*,#13407,.T.);
#17240=ORIENTED_EDGE('',*,*,#13408,.T.);
#17241=ORIENTED_EDGE('',*,*,#13389,.F.);
#17242=ORIENTED_EDGE('',*,*,#13384,.F.);
#17243=ORIENTED_EDGE('',*,*,#13388,.T.);
#17244=ORIENTED_EDGE('',*,*,#13409,.T.);
#17245=ORIENTED_EDGE('',*,*,#13407,.F.);
#17246=ORIENTED_EDGE('',*,*,#13387,.F.);
#17247=ORIENTED_EDGE('',*,*,#13390,.F.);
#17248=ORIENTED_EDGE('',*,*,#13408,.F.);
#17249=ORIENTED_EDGE('',*,*,#13409,.F.);
#17250=ORIENTED_EDGE('',*,*,#13400,.F.);
#17251=ORIENTED_EDGE('',*,*,#13403,.F.);
#17252=ORIENTED_EDGE('',*,*,#13405,.F.);
#17253=ORIENTED_EDGE('',*,*,#13406,.F.);
#17254=ORIENTED_EDGE('',*,*,#13172,.F.);
#17255=ORIENTED_EDGE('',*,*,#13410,.T.);
#17256=ORIENTED_EDGE('',*,*,#13411,.T.);
#17257=ORIENTED_EDGE('',*,*,#13410,.F.);
#17258=ORIENTED_EDGE('',*,*,#13411,.F.);
#17259=ORIENTED_EDGE('',*,*,#13173,.F.);
#17260=ORIENTED_EDGE('',*,*,#13412,.T.);
#17261=ORIENTED_EDGE('',*,*,#13413,.T.);
#17262=ORIENTED_EDGE('',*,*,#13412,.F.);
#17263=ORIENTED_EDGE('',*,*,#13413,.F.);
#17264=ORIENTED_EDGE('',*,*,#13414,.T.);
#17265=ORIENTED_EDGE('',*,*,#13415,.F.);
#17266=ORIENTED_EDGE('',*,*,#13414,.F.);
#17267=ORIENTED_EDGE('',*,*,#13416,.T.);
#17268=ORIENTED_EDGE('',*,*,#13417,.T.);
#17269=ORIENTED_EDGE('',*,*,#13416,.F.);
#17270=ORIENTED_EDGE('',*,*,#13417,.F.);
#17271=ORIENTED_EDGE('',*,*,#13418,.F.);
#17272=ORIENTED_EDGE('',*,*,#13418,.T.);
#17273=ORIENTED_EDGE('',*,*,#13419,.T.);
#17274=ORIENTED_EDGE('',*,*,#13035,.T.);
#17275=ORIENTED_EDGE('',*,*,#13419,.F.);
#17276=ORIENTED_EDGE('',*,*,#13373,.F.);
#17277=ORIENTED_EDGE('',*,*,#13420,.T.);
#17278=ORIENTED_EDGE('',*,*,#13415,.T.);
#17279=ORIENTED_EDGE('',*,*,#13420,.F.);
#17280=ORIENTED_EDGE('',*,*,#13115,.T.);
#17281=ORIENTED_EDGE('',*,*,#13111,.F.);
#17282=ORIENTED_EDGE('',*,*,#13105,.T.);
#17283=ORIENTED_EDGE('',*,*,#13049,.F.);
#17284=ORIENTED_EDGE('',*,*,#13375,.T.);
#17285=ORIENTED_EDGE('',*,*,#13347,.T.);
#17286=ORIENTED_EDGE('',*,*,#13209,.T.);
#17287=ORIENTED_EDGE('',*,*,#13205,.F.);
#17288=ORIENTED_EDGE('',*,*,#13199,.T.);
#17289=ORIENTED_EDGE('',*,*,#13193,.F.);
#17290=ORIENTED_EDGE('',*,*,#13350,.T.);
#17291=ORIENTED_EDGE('',*,*,#13351,.T.);
#17292=ORIENTED_EDGE('',*,*,#13280,.T.);
#17293=ORIENTED_EDGE('',*,*,#13297,.F.);
#17294=ORIENTED_EDGE('',*,*,#13299,.F.);
#17295=ORIENTED_EDGE('',*,*,#13301,.F.);
#17296=ORIENTED_EDGE('',*,*,#13303,.F.);
#17297=ORIENTED_EDGE('',*,*,#13305,.F.);
#17298=ORIENTED_EDGE('',*,*,#13307,.T.);
#17299=ORIENTED_EDGE('',*,*,#13309,.T.);
#17300=ORIENTED_EDGE('',*,*,#13339,.T.);
#17301=ORIENTED_EDGE('',*,*,#13225,.F.);
#17302=ORIENTED_EDGE('',*,*,#13228,.T.);
#17303=ORIENTED_EDGE('',*,*,#13213,.F.);
#17304=ORIENTED_EDGE('',*,*,#13341,.T.);
#17305=ORIENTED_EDGE('',*,*,#13274,.T.);
#17306=ORIENTED_EDGE('',*,*,#13028,.T.);
#17307=ORIENTED_EDGE('',*,*,#13022,.T.);
#17308=ORIENTED_EDGE('',*,*,#13254,.F.);
#17309=ORIENTED_EDGE('',*,*,#13265,.F.);
#17310=ORIENTED_EDGE('',*,*,#13421,.F.);
#17311=ORIENTED_EDGE('',*,*,#13422,.F.);
#17312=ORIENTED_EDGE('',*,*,#13237,.F.);
#17313=ORIENTED_EDGE('',*,*,#13248,.F.);
#17314=ORIENTED_EDGE('',*,*,#13423,.F.);
#17315=ORIENTED_EDGE('',*,*,#13424,.F.);
#17316=ORIENTED_EDGE('',*,*,#13232,.F.);
#17317=ORIENTED_EDGE('',*,*,#13425,.F.);
#17318=ORIENTED_EDGE('',*,*,#13323,.F.);
#17319=ORIENTED_EDGE('',*,*,#13426,.T.);
#17320=ORIENTED_EDGE('',*,*,#13359,.F.);
#17321=ORIENTED_EDGE('',*,*,#13336,.F.);
#17322=ORIENTED_EDGE('',*,*,#13326,.F.);
#17323=ORIENTED_EDGE('',*,*,#13233,.T.);
#17324=ORIENTED_EDGE('',*,*,#13229,.F.);
#17325=ORIENTED_EDGE('',*,*,#13425,.T.);
#17326=ORIENTED_EDGE('',*,*,#13231,.F.);
#17327=ORIENTED_EDGE('',*,*,#13235,.T.);
#17328=ORIENTED_EDGE('',*,*,#13245,.F.);
#17329=ORIENTED_EDGE('',*,*,#13424,.T.);
#17330=ORIENTED_EDGE('',*,*,#13427,.T.);
#17331=ORIENTED_EDGE('',*,*,#13251,.F.);
#17332=ORIENTED_EDGE('',*,*,#13262,.F.);
#17333=ORIENTED_EDGE('',*,*,#13422,.T.);
#17334=ORIENTED_EDGE('',*,*,#13428,.T.);
#17335=ORIENTED_EDGE('',*,*,#13268,.F.);
#17336=ORIENTED_EDGE('',*,*,#13421,.T.);
#17337=ORIENTED_EDGE('',*,*,#13264,.T.);
#17338=ORIENTED_EDGE('',*,*,#13267,.F.);
#17339=ORIENTED_EDGE('',*,*,#13269,.F.);
#17340=ORIENTED_EDGE('',*,*,#13428,.F.);
#17341=ORIENTED_EDGE('',*,*,#13423,.T.);
#17342=ORIENTED_EDGE('',*,*,#13247,.T.);
#17343=ORIENTED_EDGE('',*,*,#13250,.F.);
#17344=ORIENTED_EDGE('',*,*,#13252,.F.);
#17345=ORIENTED_EDGE('',*,*,#13427,.F.);
#17346=ORIENTED_EDGE('',*,*,#13320,.F.);
#17347=ORIENTED_EDGE('',*,*,#13329,.T.);
#17348=ORIENTED_EDGE('',*,*,#13362,.F.);
#17349=ORIENTED_EDGE('',*,*,#13429,.F.);
#17350=ORIENTED_EDGE('',*,*,#13322,.F.);
#17351=ORIENTED_EDGE('',*,*,#13429,.T.);
#17352=ORIENTED_EDGE('',*,*,#13361,.F.);
#17353=ORIENTED_EDGE('',*,*,#13426,.F.);
#17354=ORIENTED_EDGE('',*,*,#13430,.T.);
#17355=ORIENTED_EDGE('',*,*,#13431,.T.);
#17356=ORIENTED_EDGE('',*,*,#13432,.T.);
#17357=ORIENTED_EDGE('',*,*,#13431,.F.);
#17358=ORIENTED_EDGE('',*,*,#13432,.F.);
#17359=ORIENTED_EDGE('',*,*,#13433,.T.);
#17360=ORIENTED_EDGE('',*,*,#13434,.T.);
#17361=ORIENTED_EDGE('',*,*,#13433,.F.);
#17362=ORIENTED_EDGE('',*,*,#13435,.F.);
#17363=ORIENTED_EDGE('',*,*,#13430,.F.);
#17364=ORIENTED_EDGE('',*,*,#13436,.T.);
#17365=ORIENTED_EDGE('',*,*,#13437,.T.);
#17366=ORIENTED_EDGE('',*,*,#13438,.T.);
#17367=ORIENTED_EDGE('',*,*,#13437,.F.);
#17368=ORIENTED_EDGE('',*,*,#13438,.F.);
#17369=ORIENTED_EDGE('',*,*,#13439,.T.);
#17370=ORIENTED_EDGE('',*,*,#13440,.T.);
#17371=ORIENTED_EDGE('',*,*,#13439,.F.);
#17372=ORIENTED_EDGE('',*,*,#13441,.F.);
#17373=ORIENTED_EDGE('',*,*,#13436,.F.);
#17374=ORIENTED_EDGE('',*,*,#13442,.T.);
#17375=ORIENTED_EDGE('',*,*,#13443,.T.);
#17376=ORIENTED_EDGE('',*,*,#13444,.T.);
#17377=ORIENTED_EDGE('',*,*,#13445,.T.);
#17378=ORIENTED_EDGE('',*,*,#13446,.T.);
#17379=ORIENTED_EDGE('',*,*,#13447,.T.);
#17380=ORIENTED_EDGE('',*,*,#13444,.F.);
#17381=ORIENTED_EDGE('',*,*,#13448,.T.);
#17382=ORIENTED_EDGE('',*,*,#13449,.T.);
#17383=ORIENTED_EDGE('',*,*,#13450,.T.);
#17384=ORIENTED_EDGE('',*,*,#13446,.F.);
#17385=ORIENTED_EDGE('',*,*,#13451,.T.);
#17386=ORIENTED_EDGE('',*,*,#13452,.T.);
#17387=ORIENTED_EDGE('',*,*,#13453,.T.);
#17388=ORIENTED_EDGE('',*,*,#13449,.F.);
#17389=ORIENTED_EDGE('',*,*,#13454,.T.);
#17390=ORIENTED_EDGE('',*,*,#13455,.T.);
#17391=ORIENTED_EDGE('',*,*,#13456,.T.);
#17392=ORIENTED_EDGE('',*,*,#13452,.F.);
#17393=ORIENTED_EDGE('',*,*,#13457,.T.);
#17394=ORIENTED_EDGE('',*,*,#13458,.T.);
#17395=ORIENTED_EDGE('',*,*,#13459,.T.);
#17396=ORIENTED_EDGE('',*,*,#13455,.F.);
#17397=ORIENTED_EDGE('',*,*,#13460,.T.);
#17398=ORIENTED_EDGE('',*,*,#13461,.T.);
#17399=ORIENTED_EDGE('',*,*,#13462,.T.);
#17400=ORIENTED_EDGE('',*,*,#13458,.F.);
#17401=ORIENTED_EDGE('',*,*,#13463,.T.);
#17402=ORIENTED_EDGE('',*,*,#13442,.F.);
#17403=ORIENTED_EDGE('',*,*,#13464,.T.);
#17404=ORIENTED_EDGE('',*,*,#13461,.F.);
#17405=ORIENTED_EDGE('',*,*,#13465,.T.);
#17406=ORIENTED_EDGE('',*,*,#13454,.F.);
#17407=ORIENTED_EDGE('',*,*,#13466,.F.);
#17408=ORIENTED_EDGE('',*,*,#13467,.F.);
#17409=ORIENTED_EDGE('',*,*,#13468,.T.);
#17410=ORIENTED_EDGE('',*,*,#13451,.F.);
#17411=ORIENTED_EDGE('',*,*,#13469,.F.);
#17412=ORIENTED_EDGE('',*,*,#13470,.F.);
#17413=ORIENTED_EDGE('',*,*,#13466,.T.);
#17414=ORIENTED_EDGE('',*,*,#13448,.F.);
#17415=ORIENTED_EDGE('',*,*,#13471,.F.);
#17416=ORIENTED_EDGE('',*,*,#13472,.F.);
#17417=ORIENTED_EDGE('',*,*,#13469,.T.);
#17418=ORIENTED_EDGE('',*,*,#13443,.F.);
#17419=ORIENTED_EDGE('',*,*,#13473,.F.);
#17420=ORIENTED_EDGE('',*,*,#13474,.F.);
#17421=ORIENTED_EDGE('',*,*,#13471,.T.);
#17422=ORIENTED_EDGE('',*,*,#13475,.T.);
#17423=ORIENTED_EDGE('',*,*,#13445,.F.);
#17424=ORIENTED_EDGE('',*,*,#13447,.F.);
#17425=ORIENTED_EDGE('',*,*,#13450,.F.);
#17426=ORIENTED_EDGE('',*,*,#13453,.F.);
#17427=ORIENTED_EDGE('',*,*,#13456,.F.);
#17428=ORIENTED_EDGE('',*,*,#13459,.F.);
#17429=ORIENTED_EDGE('',*,*,#13462,.F.);
#17430=ORIENTED_EDGE('',*,*,#13464,.F.);
#17431=ORIENTED_EDGE('',*,*,#13476,.T.);
#17432=ORIENTED_EDGE('',*,*,#13477,.T.);
#17433=ORIENTED_EDGE('',*,*,#13478,.T.);
#17434=ORIENTED_EDGE('',*,*,#13479,.T.);
#17435=ORIENTED_EDGE('',*,*,#13480,.T.);
#17436=ORIENTED_EDGE('',*,*,#13481,.T.);
#17437=ORIENTED_EDGE('',*,*,#13482,.T.);
#17438=ORIENTED_EDGE('',*,*,#13483,.T.);
#17439=ORIENTED_EDGE('',*,*,#13484,.T.);
#17440=ORIENTED_EDGE('',*,*,#13474,.T.);
#17441=ORIENTED_EDGE('',*,*,#13485,.T.);
#17442=ORIENTED_EDGE('',*,*,#13486,.T.);
#17443=ORIENTED_EDGE('',*,*,#13487,.T.);
#17444=ORIENTED_EDGE('',*,*,#13488,.T.);
#17445=ORIENTED_EDGE('',*,*,#13485,.F.);
#17446=ORIENTED_EDGE('',*,*,#13489,.T.);
#17447=ORIENTED_EDGE('',*,*,#13490,.T.);
#17448=ORIENTED_EDGE('',*,*,#13491,.T.);
#17449=ORIENTED_EDGE('',*,*,#13487,.F.);
#17450=ORIENTED_EDGE('',*,*,#13492,.T.);
#17451=ORIENTED_EDGE('',*,*,#13493,.T.);
#17452=ORIENTED_EDGE('',*,*,#13494,.T.);
#17453=ORIENTED_EDGE('',*,*,#13490,.F.);
#17454=ORIENTED_EDGE('',*,*,#13495,.T.);
#17455=ORIENTED_EDGE('',*,*,#13496,.T.);
#17456=ORIENTED_EDGE('',*,*,#13497,.T.);
#17457=ORIENTED_EDGE('',*,*,#13493,.F.);
#17458=ORIENTED_EDGE('',*,*,#13498,.T.);
#17459=ORIENTED_EDGE('',*,*,#13499,.T.);
#17460=ORIENTED_EDGE('',*,*,#13500,.T.);
#17461=ORIENTED_EDGE('',*,*,#13496,.F.);
#17462=ORIENTED_EDGE('',*,*,#13467,.T.);
#17463=ORIENTED_EDGE('',*,*,#13501,.T.);
#17464=ORIENTED_EDGE('',*,*,#13502,.T.);
#17465=ORIENTED_EDGE('',*,*,#13499,.F.);
#17466=ORIENTED_EDGE('',*,*,#13470,.T.);
#17467=ORIENTED_EDGE('',*,*,#13501,.F.);
#17468=ORIENTED_EDGE('',*,*,#13472,.T.);
#17469=ORIENTED_EDGE('',*,*,#13484,.F.);
#17470=ORIENTED_EDGE('',*,*,#13503,.T.);
#17471=ORIENTED_EDGE('',*,*,#13460,.F.);
#17472=ORIENTED_EDGE('',*,*,#13504,.F.);
#17473=ORIENTED_EDGE('',*,*,#13495,.F.);
#17474=ORIENTED_EDGE('',*,*,#13505,.T.);
#17475=ORIENTED_EDGE('',*,*,#13463,.F.);
#17476=ORIENTED_EDGE('',*,*,#13505,.F.);
#17477=ORIENTED_EDGE('',*,*,#13492,.F.);
#17478=ORIENTED_EDGE('',*,*,#13506,.T.);
#17479=ORIENTED_EDGE('',*,*,#13465,.F.);
#17480=ORIENTED_EDGE('',*,*,#13506,.F.);
#17481=ORIENTED_EDGE('',*,*,#13489,.F.);
#17482=ORIENTED_EDGE('',*,*,#13473,.T.);
#17483=ORIENTED_EDGE('',*,*,#13486,.F.);
#17484=ORIENTED_EDGE('',*,*,#13488,.F.);
#17485=ORIENTED_EDGE('',*,*,#13491,.F.);
#17486=ORIENTED_EDGE('',*,*,#13494,.F.);
#17487=ORIENTED_EDGE('',*,*,#13497,.F.);
#17488=ORIENTED_EDGE('',*,*,#13500,.F.);
#17489=ORIENTED_EDGE('',*,*,#13502,.F.);
#17490=ORIENTED_EDGE('',*,*,#13503,.F.);
#17491=ORIENTED_EDGE('',*,*,#13507,.T.);
#17492=ORIENTED_EDGE('',*,*,#13508,.T.);
#17493=ORIENTED_EDGE('',*,*,#13509,.T.);
#17494=ORIENTED_EDGE('',*,*,#13510,.T.);
#17495=ORIENTED_EDGE('',*,*,#13511,.T.);
#17496=ORIENTED_EDGE('',*,*,#13512,.T.);
#17497=ORIENTED_EDGE('',*,*,#13513,.T.);
#17498=ORIENTED_EDGE('',*,*,#13514,.T.);
#17499=ORIENTED_EDGE('',*,*,#13476,.F.);
#17500=ORIENTED_EDGE('',*,*,#13515,.T.);
#17501=ORIENTED_EDGE('',*,*,#13516,.T.);
#17502=ORIENTED_EDGE('',*,*,#13515,.F.);
#17503=ORIENTED_EDGE('',*,*,#13516,.F.);
#17504=ORIENTED_EDGE('',*,*,#13477,.F.);
#17505=ORIENTED_EDGE('',*,*,#13517,.T.);
#17506=ORIENTED_EDGE('',*,*,#13518,.T.);
#17507=ORIENTED_EDGE('',*,*,#13517,.F.);
#17508=ORIENTED_EDGE('',*,*,#13518,.F.);
#17509=ORIENTED_EDGE('',*,*,#13507,.F.);
#17510=ORIENTED_EDGE('',*,*,#13519,.T.);
#17511=ORIENTED_EDGE('',*,*,#13520,.T.);
#17512=ORIENTED_EDGE('',*,*,#13519,.F.);
#17513=ORIENTED_EDGE('',*,*,#13520,.F.);
#17514=ORIENTED_EDGE('',*,*,#13508,.F.);
#17515=ORIENTED_EDGE('',*,*,#13521,.T.);
#17516=ORIENTED_EDGE('',*,*,#13522,.T.);
#17517=ORIENTED_EDGE('',*,*,#13521,.F.);
#17518=ORIENTED_EDGE('',*,*,#13522,.F.);
#17519=ORIENTED_EDGE('',*,*,#13514,.F.);
#17520=ORIENTED_EDGE('',*,*,#13523,.T.);
#17521=ORIENTED_EDGE('',*,*,#13483,.F.);
#17522=ORIENTED_EDGE('',*,*,#13523,.F.);
#17523=ORIENTED_EDGE('',*,*,#13513,.F.);
#17524=ORIENTED_EDGE('',*,*,#13524,.T.);
#17525=ORIENTED_EDGE('',*,*,#13482,.F.);
#17526=ORIENTED_EDGE('',*,*,#13524,.F.);
#17527=ORIENTED_EDGE('',*,*,#13512,.F.);
#17528=ORIENTED_EDGE('',*,*,#13525,.T.);
#17529=ORIENTED_EDGE('',*,*,#13481,.F.);
#17530=ORIENTED_EDGE('',*,*,#13525,.F.);
#17531=ORIENTED_EDGE('',*,*,#13511,.F.);
#17532=ORIENTED_EDGE('',*,*,#13526,.T.);
#17533=ORIENTED_EDGE('',*,*,#13480,.F.);
#17534=ORIENTED_EDGE('',*,*,#13526,.F.);
#17535=ORIENTED_EDGE('',*,*,#13527,.F.);
#17536=ORIENTED_EDGE('',*,*,#13528,.T.);
#17537=ORIENTED_EDGE('',*,*,#13529,.F.);
#17538=ORIENTED_EDGE('',*,*,#13530,.F.);
#17539=ORIENTED_EDGE('',*,*,#13531,.F.);
#17540=ORIENTED_EDGE('',*,*,#13528,.F.);
#17541=ORIENTED_EDGE('',*,*,#13529,.T.);
#17542=ORIENTED_EDGE('',*,*,#13531,.T.);
#17543=ORIENTED_EDGE('',*,*,#13532,.T.);
#17544=ORIENTED_EDGE('',*,*,#13478,.F.);
#17545=ORIENTED_EDGE('',*,*,#13533,.F.);
#17546=ORIENTED_EDGE('',*,*,#13534,.T.);
#17547=ORIENTED_EDGE('',*,*,#13535,.T.);
#17548=ORIENTED_EDGE('',*,*,#13536,.F.);
#17549=ORIENTED_EDGE('',*,*,#13509,.F.);
#17550=ORIENTED_EDGE('',*,*,#13537,.T.);
#17551=ORIENTED_EDGE('',*,*,#13440,.F.);
#17552=ORIENTED_EDGE('',*,*,#13527,.T.);
#17553=ORIENTED_EDGE('',*,*,#13538,.F.);
#17554=ORIENTED_EDGE('',*,*,#13539,.T.);
#17555=ORIENTED_EDGE('',*,*,#13441,.T.);
#17556=ORIENTED_EDGE('',*,*,#13539,.F.);
#17557=ORIENTED_EDGE('',*,*,#13540,.F.);
#17558=ORIENTED_EDGE('',*,*,#13541,.T.);
#17559=ORIENTED_EDGE('',*,*,#13534,.F.);
#17560=ORIENTED_EDGE('',*,*,#13542,.F.);
#17561=ORIENTED_EDGE('',*,*,#13535,.F.);
#17562=ORIENTED_EDGE('',*,*,#13541,.F.);
#17563=ORIENTED_EDGE('',*,*,#13530,.T.);
#17564=ORIENTED_EDGE('',*,*,#13537,.F.);
#17565=ORIENTED_EDGE('',*,*,#13510,.F.);
#17566=ORIENTED_EDGE('',*,*,#13536,.T.);
#17567=ORIENTED_EDGE('',*,*,#13542,.T.);
#17568=ORIENTED_EDGE('',*,*,#13533,.T.);
#17569=ORIENTED_EDGE('',*,*,#13479,.F.);
#17570=ORIENTED_EDGE('',*,*,#13532,.F.);
#17571=ORIENTED_EDGE('',*,*,#13434,.F.);
#17572=ORIENTED_EDGE('',*,*,#13540,.T.);
#17573=ORIENTED_EDGE('',*,*,#13475,.F.);
#17574=ORIENTED_EDGE('',*,*,#13543,.T.);
#17575=ORIENTED_EDGE('',*,*,#13435,.T.);
#17576=ORIENTED_EDGE('',*,*,#13543,.F.);
#17577=ORIENTED_EDGE('',*,*,#13457,.F.);
#17578=ORIENTED_EDGE('',*,*,#13468,.F.);
#17579=ORIENTED_EDGE('',*,*,#13498,.F.);
#17580=ORIENTED_EDGE('',*,*,#13504,.T.);
#17581=ORIENTED_EDGE('',*,*,#13538,.T.);
#17582=ORIENTED_EDGE('',*,*,#13544,.T.);
#17583=ORIENTED_EDGE('',*,*,#13545,.T.);
#17584=ORIENTED_EDGE('',*,*,#13546,.T.);
#17585=ORIENTED_EDGE('',*,*,#13545,.F.);
#17586=ORIENTED_EDGE('',*,*,#13547,.F.);
#17587=ORIENTED_EDGE('',*,*,#13546,.F.);
#17588=ORIENTED_EDGE('',*,*,#13544,.F.);
#17589=ORIENTED_EDGE('',*,*,#13548,.T.);
#17590=ORIENTED_EDGE('',*,*,#13549,.T.);
#17591=ORIENTED_EDGE('',*,*,#13548,.F.);
#17592=ORIENTED_EDGE('',*,*,#13550,.T.);
#17593=ORIENTED_EDGE('',*,*,#13551,.T.);
#17594=ORIENTED_EDGE('',*,*,#13552,.T.);
#17595=ORIENTED_EDGE('',*,*,#13553,.T.);
#17596=ORIENTED_EDGE('',*,*,#13554,.T.);
#17597=ORIENTED_EDGE('',*,*,#13555,.T.);
#17598=ORIENTED_EDGE('',*,*,#13550,.F.);
#17599=ORIENTED_EDGE('',*,*,#13556,.T.);
#17600=ORIENTED_EDGE('',*,*,#13557,.T.);
#17601=ORIENTED_EDGE('',*,*,#13558,.T.);
#17602=ORIENTED_EDGE('',*,*,#13554,.F.);
#17603=ORIENTED_EDGE('',*,*,#13559,.T.);
#17604=ORIENTED_EDGE('',*,*,#13552,.F.);
#17605=ORIENTED_EDGE('',*,*,#13560,.T.);
#17606=ORIENTED_EDGE('',*,*,#13557,.F.);
#17607=ORIENTED_EDGE('',*,*,#13561,.T.);
#17608=ORIENTED_EDGE('',*,*,#13556,.F.);
#17609=ORIENTED_EDGE('',*,*,#13562,.T.);
#17610=ORIENTED_EDGE('',*,*,#13563,.T.);
#17611=ORIENTED_EDGE('',*,*,#13564,.F.);
#17612=ORIENTED_EDGE('',*,*,#13553,.F.);
#17613=ORIENTED_EDGE('',*,*,#13565,.T.);
#17614=ORIENTED_EDGE('',*,*,#13566,.T.);
#17615=ORIENTED_EDGE('',*,*,#13562,.F.);
#17616=ORIENTED_EDGE('',*,*,#13567,.F.);
#17617=ORIENTED_EDGE('',*,*,#13568,.F.);
#17618=ORIENTED_EDGE('',*,*,#13569,.F.);
#17619=ORIENTED_EDGE('',*,*,#13570,.F.);
#17620=ORIENTED_EDGE('',*,*,#13571,.F.);
#17621=ORIENTED_EDGE('',*,*,#13572,.F.);
#17622=ORIENTED_EDGE('',*,*,#13573,.F.);
#17623=ORIENTED_EDGE('',*,*,#13574,.F.);
#17624=ORIENTED_EDGE('',*,*,#13575,.T.);
#17625=ORIENTED_EDGE('',*,*,#13576,.T.);
#17626=ORIENTED_EDGE('',*,*,#13577,.T.);
#17627=ORIENTED_EDGE('',*,*,#13578,.T.);
#17628=ORIENTED_EDGE('',*,*,#13579,.T.);
#17629=ORIENTED_EDGE('',*,*,#13580,.T.);
#17630=ORIENTED_EDGE('',*,*,#13551,.F.);
#17631=ORIENTED_EDGE('',*,*,#13555,.F.);
#17632=ORIENTED_EDGE('',*,*,#13558,.F.);
#17633=ORIENTED_EDGE('',*,*,#13560,.F.);
#17634=ORIENTED_EDGE('',*,*,#13581,.T.);
#17635=ORIENTED_EDGE('',*,*,#13582,.T.);
#17636=ORIENTED_EDGE('',*,*,#13583,.T.);
#17637=ORIENTED_EDGE('',*,*,#13584,.T.);
#17638=ORIENTED_EDGE('',*,*,#13585,.T.);
#17639=ORIENTED_EDGE('',*,*,#13586,.T.);
#17640=ORIENTED_EDGE('',*,*,#13581,.F.);
#17641=ORIENTED_EDGE('',*,*,#13587,.T.);
#17642=ORIENTED_EDGE('',*,*,#13588,.T.);
#17643=ORIENTED_EDGE('',*,*,#13589,.T.);
#17644=ORIENTED_EDGE('',*,*,#13585,.F.);
#17645=ORIENTED_EDGE('',*,*,#13590,.T.);
#17646=ORIENTED_EDGE('',*,*,#13583,.F.);
#17647=ORIENTED_EDGE('',*,*,#13591,.T.);
#17648=ORIENTED_EDGE('',*,*,#13588,.F.);
#17649=ORIENTED_EDGE('',*,*,#13592,.T.);
#17650=ORIENTED_EDGE('',*,*,#13587,.F.);
#17651=ORIENTED_EDGE('',*,*,#13593,.T.);
#17652=ORIENTED_EDGE('',*,*,#13594,.T.);
#17653=ORIENTED_EDGE('',*,*,#13595,.F.);
#17654=ORIENTED_EDGE('',*,*,#13584,.F.);
#17655=ORIENTED_EDGE('',*,*,#13596,.T.);
#17656=ORIENTED_EDGE('',*,*,#13597,.T.);
#17657=ORIENTED_EDGE('',*,*,#13593,.F.);
#17658=ORIENTED_EDGE('',*,*,#13582,.F.);
#17659=ORIENTED_EDGE('',*,*,#13586,.F.);
#17660=ORIENTED_EDGE('',*,*,#13589,.F.);
#17661=ORIENTED_EDGE('',*,*,#13591,.F.);
#17662=ORIENTED_EDGE('',*,*,#13598,.T.);
#17663=ORIENTED_EDGE('',*,*,#13599,.T.);
#17664=ORIENTED_EDGE('',*,*,#13600,.T.);
#17665=ORIENTED_EDGE('',*,*,#13599,.F.);
#17666=ORIENTED_EDGE('',*,*,#13601,.T.);
#17667=ORIENTED_EDGE('',*,*,#13602,.T.);
#17668=ORIENTED_EDGE('',*,*,#13598,.F.);
#17669=ORIENTED_EDGE('',*,*,#13603,.T.);
#17670=ORIENTED_EDGE('',*,*,#13604,.F.);
#17671=ORIENTED_EDGE('',*,*,#13605,.F.);
#17672=ORIENTED_EDGE('',*,*,#13606,.T.);
#17673=ORIENTED_EDGE('',*,*,#13607,.F.);
#17674=ORIENTED_EDGE('',*,*,#13608,.F.);
#17675=ORIENTED_EDGE('',*,*,#13609,.T.);
#17676=ORIENTED_EDGE('',*,*,#13610,.T.);
#17677=ORIENTED_EDGE('',*,*,#13601,.F.);
#17678=ORIENTED_EDGE('',*,*,#13600,.F.);
#17679=ORIENTED_EDGE('',*,*,#13611,.T.);
#17680=ORIENTED_EDGE('',*,*,#13612,.T.);
#17681=ORIENTED_EDGE('',*,*,#13611,.F.);
#17682=ORIENTED_EDGE('',*,*,#13605,.T.);
#17683=ORIENTED_EDGE('',*,*,#13613,.T.);
#17684=ORIENTED_EDGE('',*,*,#13614,.T.);
#17685=ORIENTED_EDGE('',*,*,#13613,.F.);
#17686=ORIENTED_EDGE('',*,*,#13604,.T.);
#17687=ORIENTED_EDGE('',*,*,#13615,.T.);
#17688=ORIENTED_EDGE('',*,*,#13614,.F.);
#17689=ORIENTED_EDGE('',*,*,#13616,.T.);
#17690=ORIENTED_EDGE('',*,*,#13617,.T.);
#17691=ORIENTED_EDGE('',*,*,#13616,.F.);
#17692=ORIENTED_EDGE('',*,*,#13618,.T.);
#17693=ORIENTED_EDGE('',*,*,#13619,.T.);
#17694=ORIENTED_EDGE('',*,*,#13620,.T.);
#17695=ORIENTED_EDGE('',*,*,#13621,.T.);
#17696=ORIENTED_EDGE('',*,*,#13619,.F.);
#17697=ORIENTED_EDGE('',*,*,#13622,.T.);
#17698=ORIENTED_EDGE('',*,*,#13623,.T.);
#17699=ORIENTED_EDGE('',*,*,#13618,.F.);
#17700=ORIENTED_EDGE('',*,*,#13624,.T.);
#17701=ORIENTED_EDGE('',*,*,#13625,.F.);
#17702=ORIENTED_EDGE('',*,*,#13626,.F.);
#17703=ORIENTED_EDGE('',*,*,#13627,.T.);
#17704=ORIENTED_EDGE('',*,*,#13628,.T.);
#17705=ORIENTED_EDGE('',*,*,#13629,.F.);
#17706=ORIENTED_EDGE('',*,*,#13630,.T.);
#17707=ORIENTED_EDGE('',*,*,#13631,.T.);
#17708=ORIENTED_EDGE('',*,*,#13622,.F.);
#17709=ORIENTED_EDGE('',*,*,#13620,.F.);
#17710=ORIENTED_EDGE('',*,*,#13621,.F.);
#17711=ORIENTED_EDGE('',*,*,#13632,.T.);
#17712=ORIENTED_EDGE('',*,*,#13633,.T.);
#17713=ORIENTED_EDGE('',*,*,#13632,.F.);
#17714=ORIENTED_EDGE('',*,*,#13626,.T.);
#17715=ORIENTED_EDGE('',*,*,#13634,.T.);
#17716=ORIENTED_EDGE('',*,*,#13635,.T.);
#17717=ORIENTED_EDGE('',*,*,#13636,.T.);
#17718=ORIENTED_EDGE('',*,*,#13634,.F.);
#17719=ORIENTED_EDGE('',*,*,#13625,.T.);
#17720=ORIENTED_EDGE('',*,*,#13637,.T.);
#17721=ORIENTED_EDGE('',*,*,#13635,.F.);
#17722=ORIENTED_EDGE('',*,*,#13636,.F.);
#17723=ORIENTED_EDGE('',*,*,#13638,.T.);
#17724=ORIENTED_EDGE('',*,*,#13639,.T.);
#17725=ORIENTED_EDGE('',*,*,#13638,.F.);
#17726=ORIENTED_EDGE('',*,*,#13640,.T.);
#17727=ORIENTED_EDGE('',*,*,#13641,.T.);
#17728=ORIENTED_EDGE('',*,*,#13642,.T.);
#17729=ORIENTED_EDGE('',*,*,#13567,.T.);
#17730=ORIENTED_EDGE('',*,*,#13640,.F.);
#17731=ORIENTED_EDGE('',*,*,#13574,.T.);
#17732=ORIENTED_EDGE('',*,*,#13643,.T.);
#17733=ORIENTED_EDGE('',*,*,#13644,.T.);
#17734=ORIENTED_EDGE('',*,*,#13645,.T.);
#17735=ORIENTED_EDGE('',*,*,#13646,.T.);
#17736=ORIENTED_EDGE('',*,*,#13643,.F.);
#17737=ORIENTED_EDGE('',*,*,#13573,.T.);
#17738=ORIENTED_EDGE('',*,*,#13645,.F.);
#17739=ORIENTED_EDGE('',*,*,#13572,.T.);
#17740=ORIENTED_EDGE('',*,*,#13647,.T.);
#17741=ORIENTED_EDGE('',*,*,#13648,.T.);
#17742=ORIENTED_EDGE('',*,*,#13649,.T.);
#17743=ORIENTED_EDGE('',*,*,#13650,.T.);
#17744=ORIENTED_EDGE('',*,*,#13647,.F.);
#17745=ORIENTED_EDGE('',*,*,#13571,.T.);
#17746=ORIENTED_EDGE('',*,*,#13649,.F.);
#17747=ORIENTED_EDGE('',*,*,#13570,.T.);
#17748=ORIENTED_EDGE('',*,*,#13651,.T.);
#17749=ORIENTED_EDGE('',*,*,#13652,.T.);
#17750=ORIENTED_EDGE('',*,*,#13653,.T.);
#17751=ORIENTED_EDGE('',*,*,#13654,.T.);
#17752=ORIENTED_EDGE('',*,*,#13651,.F.);
#17753=ORIENTED_EDGE('',*,*,#13569,.T.);
#17754=ORIENTED_EDGE('',*,*,#13653,.F.);
#17755=ORIENTED_EDGE('',*,*,#13568,.T.);
#17756=ORIENTED_EDGE('',*,*,#13642,.F.);
#17757=ORIENTED_EDGE('',*,*,#13655,.T.);
#17758=ORIENTED_EDGE('',*,*,#13652,.F.);
#17759=ORIENTED_EDGE('',*,*,#13656,.T.);
#17760=ORIENTED_EDGE('',*,*,#13657,.F.);
#17761=ORIENTED_EDGE('',*,*,#13658,.F.);
#17762=ORIENTED_EDGE('',*,*,#13654,.F.);
#17763=ORIENTED_EDGE('',*,*,#13659,.T.);
#17764=ORIENTED_EDGE('',*,*,#13660,.F.);
#17765=ORIENTED_EDGE('',*,*,#13656,.F.);
#17766=ORIENTED_EDGE('',*,*,#13655,.F.);
#17767=ORIENTED_EDGE('',*,*,#13661,.T.);
#17768=ORIENTED_EDGE('',*,*,#13662,.F.);
#17769=ORIENTED_EDGE('',*,*,#13659,.F.);
#17770=ORIENTED_EDGE('',*,*,#13641,.F.);
#17771=ORIENTED_EDGE('',*,*,#13663,.T.);
#17772=ORIENTED_EDGE('',*,*,#13664,.F.);
#17773=ORIENTED_EDGE('',*,*,#13661,.F.);
#17774=ORIENTED_EDGE('',*,*,#13665,.T.);
#17775=ORIENTED_EDGE('',*,*,#13629,.T.);
#17776=ORIENTED_EDGE('',*,*,#13666,.T.);
#17777=ORIENTED_EDGE('',*,*,#13657,.T.);
#17778=ORIENTED_EDGE('',*,*,#13667,.T.);
#17779=ORIENTED_EDGE('',*,*,#13668,.T.);
#17780=ORIENTED_EDGE('',*,*,#13665,.F.);
#17781=ORIENTED_EDGE('',*,*,#13660,.T.);
#17782=ORIENTED_EDGE('',*,*,#13669,.T.);
#17783=ORIENTED_EDGE('',*,*,#13670,.T.);
#17784=ORIENTED_EDGE('',*,*,#13667,.F.);
#17785=ORIENTED_EDGE('',*,*,#13662,.T.);
#17786=ORIENTED_EDGE('',*,*,#13671,.T.);
#17787=ORIENTED_EDGE('',*,*,#13672,.T.);
#17788=ORIENTED_EDGE('',*,*,#13669,.F.);
#17789=ORIENTED_EDGE('',*,*,#13664,.T.);
#17790=ORIENTED_EDGE('',*,*,#13673,.T.);
#17791=ORIENTED_EDGE('',*,*,#13608,.T.);
#17792=ORIENTED_EDGE('',*,*,#13671,.F.);
#17793=ORIENTED_EDGE('',*,*,#13674,.T.);
#17794=ORIENTED_EDGE('',*,*,#13675,.T.);
#17795=ORIENTED_EDGE('',*,*,#13676,.T.);
#17796=ORIENTED_EDGE('',*,*,#13673,.F.);
#17797=ORIENTED_EDGE('',*,*,#13677,.T.);
#17798=ORIENTED_EDGE('',*,*,#13678,.T.);
#17799=ORIENTED_EDGE('',*,*,#13679,.T.);
#17800=ORIENTED_EDGE('',*,*,#13675,.F.);
#17801=ORIENTED_EDGE('',*,*,#13680,.T.);
#17802=ORIENTED_EDGE('',*,*,#13666,.F.);
#17803=ORIENTED_EDGE('',*,*,#13681,.T.);
#17804=ORIENTED_EDGE('',*,*,#13678,.F.);
#17805=ORIENTED_EDGE('',*,*,#13682,.T.);
#17806=ORIENTED_EDGE('',*,*,#13676,.F.);
#17807=ORIENTED_EDGE('',*,*,#13683,.T.);
#17808=ORIENTED_EDGE('',*,*,#13684,.T.);
#17809=ORIENTED_EDGE('',*,*,#13609,.F.);
#17810=ORIENTED_EDGE('',*,*,#13679,.F.);
#17811=ORIENTED_EDGE('',*,*,#13685,.T.);
#17812=ORIENTED_EDGE('',*,*,#13686,.T.);
#17813=ORIENTED_EDGE('',*,*,#13683,.F.);
#17814=ORIENTED_EDGE('',*,*,#13681,.F.);
#17815=ORIENTED_EDGE('',*,*,#13628,.F.);
#17816=ORIENTED_EDGE('',*,*,#13687,.T.);
#17817=ORIENTED_EDGE('',*,*,#13685,.F.);
#17818=ORIENTED_EDGE('',*,*,#13668,.F.);
#17819=ORIENTED_EDGE('',*,*,#13688,.T.);
#17820=ORIENTED_EDGE('',*,*,#13689,.T.);
#17821=ORIENTED_EDGE('',*,*,#13630,.F.);
#17822=ORIENTED_EDGE('',*,*,#13670,.F.);
#17823=ORIENTED_EDGE('',*,*,#13690,.T.);
#17824=ORIENTED_EDGE('',*,*,#13691,.T.);
#17825=ORIENTED_EDGE('',*,*,#13688,.F.);
#17826=ORIENTED_EDGE('',*,*,#13672,.F.);
#17827=ORIENTED_EDGE('',*,*,#13607,.T.);
#17828=ORIENTED_EDGE('',*,*,#13692,.T.);
#17829=ORIENTED_EDGE('',*,*,#13690,.F.);
#17830=ORIENTED_EDGE('',*,*,#13602,.F.);
#17831=ORIENTED_EDGE('',*,*,#13610,.F.);
#17832=ORIENTED_EDGE('',*,*,#13684,.F.);
#17833=ORIENTED_EDGE('',*,*,#13686,.F.);
#17834=ORIENTED_EDGE('',*,*,#13687,.F.);
#17835=ORIENTED_EDGE('',*,*,#13627,.F.);
#17836=ORIENTED_EDGE('',*,*,#13637,.F.);
#17837=ORIENTED_EDGE('',*,*,#13624,.F.);
#17838=ORIENTED_EDGE('',*,*,#13623,.F.);
#17839=ORIENTED_EDGE('',*,*,#13631,.F.);
#17840=ORIENTED_EDGE('',*,*,#13689,.F.);
#17841=ORIENTED_EDGE('',*,*,#13691,.F.);
#17842=ORIENTED_EDGE('',*,*,#13692,.F.);
#17843=ORIENTED_EDGE('',*,*,#13606,.F.);
#17844=ORIENTED_EDGE('',*,*,#13615,.F.);
#17845=ORIENTED_EDGE('',*,*,#13603,.F.);
#17846=ORIENTED_EDGE('',*,*,#13693,.T.);
#17847=ORIENTED_EDGE('',*,*,#13592,.F.);
#17848=ORIENTED_EDGE('',*,*,#13694,.T.);
#17849=ORIENTED_EDGE('',*,*,#13695,.T.);
#17850=ORIENTED_EDGE('',*,*,#13596,.F.);
#17851=ORIENTED_EDGE('',*,*,#13590,.F.);
#17852=ORIENTED_EDGE('',*,*,#13595,.T.);
#17853=ORIENTED_EDGE('',*,*,#13696,.T.);
#17854=ORIENTED_EDGE('',*,*,#13694,.F.);
#17855=ORIENTED_EDGE('',*,*,#13561,.F.);
#17856=ORIENTED_EDGE('',*,*,#13697,.T.);
#17857=ORIENTED_EDGE('',*,*,#13698,.T.);
#17858=ORIENTED_EDGE('',*,*,#13565,.F.);
#17859=ORIENTED_EDGE('',*,*,#13559,.F.);
#17860=ORIENTED_EDGE('',*,*,#13564,.T.);
#17861=ORIENTED_EDGE('',*,*,#13699,.T.);
#17862=ORIENTED_EDGE('',*,*,#13697,.F.);
#17863=ORIENTED_EDGE('',*,*,#13563,.F.);
#17864=ORIENTED_EDGE('',*,*,#13566,.F.);
#17865=ORIENTED_EDGE('',*,*,#13698,.F.);
#17866=ORIENTED_EDGE('',*,*,#13699,.F.);
#17867=ORIENTED_EDGE('',*,*,#13594,.F.);
#17868=ORIENTED_EDGE('',*,*,#13597,.F.);
#17869=ORIENTED_EDGE('',*,*,#13695,.F.);
#17870=ORIENTED_EDGE('',*,*,#13696,.F.);
#17871=ORIENTED_EDGE('',*,*,#13693,.F.);
#17872=ORIENTED_EDGE('',*,*,#13700,.T.);
#17873=ORIENTED_EDGE('',*,*,#13547,.T.);
#17874=ORIENTED_EDGE('',*,*,#13700,.F.);
#17875=ORIENTED_EDGE('',*,*,#13549,.F.);
#17876=ORIENTED_EDGE('',*,*,#13580,.F.);
#17877=ORIENTED_EDGE('',*,*,#13701,.T.);
#17878=ORIENTED_EDGE('',*,*,#13702,.T.);
#17879=ORIENTED_EDGE('',*,*,#13701,.F.);
#17880=ORIENTED_EDGE('',*,*,#13702,.F.);
#17881=ORIENTED_EDGE('',*,*,#13579,.F.);
#17882=ORIENTED_EDGE('',*,*,#13703,.T.);
#17883=ORIENTED_EDGE('',*,*,#13704,.T.);
#17884=ORIENTED_EDGE('',*,*,#13703,.F.);
#17885=ORIENTED_EDGE('',*,*,#13704,.F.);
#17886=ORIENTED_EDGE('',*,*,#13705,.F.);
#17887=ORIENTED_EDGE('',*,*,#13706,.T.);
#17888=ORIENTED_EDGE('',*,*,#13578,.F.);
#17889=ORIENTED_EDGE('',*,*,#13706,.F.);
#17890=ORIENTED_EDGE('',*,*,#13707,.F.);
#17891=ORIENTED_EDGE('',*,*,#13708,.T.);
#17892=ORIENTED_EDGE('',*,*,#13577,.F.);
#17893=ORIENTED_EDGE('',*,*,#13708,.F.);
#17894=ORIENTED_EDGE('',*,*,#13709,.F.);
#17895=ORIENTED_EDGE('',*,*,#13710,.T.);
#17896=ORIENTED_EDGE('',*,*,#13576,.F.);
#17897=ORIENTED_EDGE('',*,*,#13710,.F.);
#17898=ORIENTED_EDGE('',*,*,#13711,.F.);
#17899=ORIENTED_EDGE('',*,*,#13712,.T.);
#17900=ORIENTED_EDGE('',*,*,#13575,.F.);
#17901=ORIENTED_EDGE('',*,*,#13712,.F.);
#17902=ORIENTED_EDGE('',*,*,#13633,.F.);
#17903=ORIENTED_EDGE('',*,*,#13705,.T.);
#17904=ORIENTED_EDGE('',*,*,#13612,.F.);
#17905=ORIENTED_EDGE('',*,*,#13707,.T.);
#17906=ORIENTED_EDGE('',*,*,#13639,.F.);
#17907=ORIENTED_EDGE('',*,*,#13709,.T.);
#17908=ORIENTED_EDGE('',*,*,#13617,.F.);
#17909=ORIENTED_EDGE('',*,*,#13711,.T.);
#17910=ORIENTED_EDGE('',*,*,#13650,.F.);
#17911=ORIENTED_EDGE('',*,*,#13658,.T.);
#17912=ORIENTED_EDGE('',*,*,#13682,.F.);
#17913=ORIENTED_EDGE('',*,*,#13713,.F.);
#17914=ORIENTED_EDGE('',*,*,#13648,.F.);
#17915=ORIENTED_EDGE('',*,*,#13713,.T.);
#17916=ORIENTED_EDGE('',*,*,#13680,.F.);
#17917=ORIENTED_EDGE('',*,*,#13714,.F.);
#17918=ORIENTED_EDGE('',*,*,#13646,.F.);
#17919=ORIENTED_EDGE('',*,*,#13714,.T.);
#17920=ORIENTED_EDGE('',*,*,#13677,.F.);
#17921=ORIENTED_EDGE('',*,*,#13715,.F.);
#17922=ORIENTED_EDGE('',*,*,#13644,.F.);
#17923=ORIENTED_EDGE('',*,*,#13715,.T.);
#17924=ORIENTED_EDGE('',*,*,#13674,.F.);
#17925=ORIENTED_EDGE('',*,*,#13663,.F.);
#17926=ORIENTED_EDGE('',*,*,#13716,.T.);
#17927=ORIENTED_EDGE('',*,*,#13717,.T.);
#17928=ORIENTED_EDGE('',*,*,#13718,.T.);
#17929=ORIENTED_EDGE('',*,*,#13719,.T.);
#17930=ORIENTED_EDGE('',*,*,#13720,.T.);
#17931=ORIENTED_EDGE('',*,*,#13721,.T.);
#17932=ORIENTED_EDGE('',*,*,#13722,.T.);
#17933=ORIENTED_EDGE('',*,*,#13717,.F.);
#17934=ORIENTED_EDGE('',*,*,#13723,.T.);
#17935=ORIENTED_EDGE('',*,*,#13724,.T.);
#17936=ORIENTED_EDGE('',*,*,#13725,.T.);
#17937=ORIENTED_EDGE('',*,*,#13726,.T.);
#17938=ORIENTED_EDGE('',*,*,#13727,.T.);
#17939=ORIENTED_EDGE('',*,*,#13728,.T.);
#17940=ORIENTED_EDGE('',*,*,#13729,.T.);
#17941=ORIENTED_EDGE('',*,*,#13730,.T.);
#17942=ORIENTED_EDGE('',*,*,#13731,.T.);
#17943=ORIENTED_EDGE('',*,*,#13732,.T.);
#17944=ORIENTED_EDGE('',*,*,#13733,.T.);
#17945=ORIENTED_EDGE('',*,*,#13734,.T.);
#17946=ORIENTED_EDGE('',*,*,#13735,.T.);
#17947=ORIENTED_EDGE('',*,*,#13736,.T.);
#17948=ORIENTED_EDGE('',*,*,#13737,.T.);
#17949=ORIENTED_EDGE('',*,*,#13738,.T.);
#17950=ORIENTED_EDGE('',*,*,#13739,.F.);
#17951=ORIENTED_EDGE('',*,*,#13740,.T.);
#17952=ORIENTED_EDGE('',*,*,#13741,.T.);
#17953=ORIENTED_EDGE('',*,*,#13742,.F.);
#17954=ORIENTED_EDGE('',*,*,#13743,.T.);
#17955=ORIENTED_EDGE('',*,*,#13744,.T.);
#17956=ORIENTED_EDGE('',*,*,#13745,.T.);
#17957=ORIENTED_EDGE('',*,*,#13746,.T.);
#17958=ORIENTED_EDGE('',*,*,#13747,.T.);
#17959=ORIENTED_EDGE('',*,*,#13748,.T.);
#17960=ORIENTED_EDGE('',*,*,#13749,.T.);
#17961=ORIENTED_EDGE('',*,*,#13750,.T.);
#17962=ORIENTED_EDGE('',*,*,#13751,.T.);
#17963=ORIENTED_EDGE('',*,*,#13752,.T.);
#17964=ORIENTED_EDGE('',*,*,#13753,.T.);
#17965=ORIENTED_EDGE('',*,*,#13754,.T.);
#17966=ORIENTED_EDGE('',*,*,#13755,.T.);
#17967=ORIENTED_EDGE('',*,*,#13756,.T.);
#17968=ORIENTED_EDGE('',*,*,#13757,.T.);
#17969=ORIENTED_EDGE('',*,*,#13758,.T.);
#17970=ORIENTED_EDGE('',*,*,#13759,.F.);
#17971=ORIENTED_EDGE('',*,*,#13760,.T.);
#17972=ORIENTED_EDGE('',*,*,#13761,.T.);
#17973=ORIENTED_EDGE('',*,*,#13762,.F.);
#17974=ORIENTED_EDGE('',*,*,#13763,.T.);
#17975=ORIENTED_EDGE('',*,*,#13764,.T.);
#17976=ORIENTED_EDGE('',*,*,#13765,.T.);
#17977=ORIENTED_EDGE('',*,*,#13766,.T.);
#17978=ORIENTED_EDGE('',*,*,#13767,.T.);
#17979=ORIENTED_EDGE('',*,*,#13768,.T.);
#17980=ORIENTED_EDGE('',*,*,#13769,.T.);
#17981=ORIENTED_EDGE('',*,*,#13770,.T.);
#17982=ORIENTED_EDGE('',*,*,#13771,.T.);
#17983=ORIENTED_EDGE('',*,*,#13772,.T.);
#17984=ORIENTED_EDGE('',*,*,#13773,.T.);
#17985=ORIENTED_EDGE('',*,*,#13774,.T.);
#17986=ORIENTED_EDGE('',*,*,#13775,.T.);
#17987=ORIENTED_EDGE('',*,*,#13776,.T.);
#17988=ORIENTED_EDGE('',*,*,#13777,.T.);
#17989=ORIENTED_EDGE('',*,*,#13778,.T.);
#17990=ORIENTED_EDGE('',*,*,#13779,.F.);
#17991=ORIENTED_EDGE('',*,*,#13780,.T.);
#17992=ORIENTED_EDGE('',*,*,#13781,.T.);
#17993=ORIENTED_EDGE('',*,*,#13782,.F.);
#17994=ORIENTED_EDGE('',*,*,#13783,.T.);
#17995=ORIENTED_EDGE('',*,*,#13784,.T.);
#17996=ORIENTED_EDGE('',*,*,#13785,.T.);
#17997=ORIENTED_EDGE('',*,*,#13786,.T.);
#17998=ORIENTED_EDGE('',*,*,#13787,.T.);
#17999=ORIENTED_EDGE('',*,*,#13788,.T.);
#18000=ORIENTED_EDGE('',*,*,#13789,.T.);
#18001=ORIENTED_EDGE('',*,*,#13790,.T.);
#18002=ORIENTED_EDGE('',*,*,#13791,.T.);
#18003=ORIENTED_EDGE('',*,*,#13792,.T.);
#18004=ORIENTED_EDGE('',*,*,#13793,.T.);
#18005=ORIENTED_EDGE('',*,*,#13794,.T.);
#18006=ORIENTED_EDGE('',*,*,#13795,.T.);
#18007=ORIENTED_EDGE('',*,*,#13796,.T.);
#18008=ORIENTED_EDGE('',*,*,#13797,.T.);
#18009=ORIENTED_EDGE('',*,*,#13798,.T.);
#18010=ORIENTED_EDGE('',*,*,#13799,.F.);
#18011=ORIENTED_EDGE('',*,*,#13800,.T.);
#18012=ORIENTED_EDGE('',*,*,#13801,.T.);
#18013=ORIENTED_EDGE('',*,*,#13802,.F.);
#18014=ORIENTED_EDGE('',*,*,#13803,.T.);
#18015=ORIENTED_EDGE('',*,*,#13804,.T.);
#18016=ORIENTED_EDGE('',*,*,#13805,.T.);
#18017=ORIENTED_EDGE('',*,*,#13806,.T.);
#18018=ORIENTED_EDGE('',*,*,#13807,.T.);
#18019=ORIENTED_EDGE('',*,*,#13808,.T.);
#18020=ORIENTED_EDGE('',*,*,#13809,.T.);
#18021=ORIENTED_EDGE('',*,*,#13810,.T.);
#18022=ORIENTED_EDGE('',*,*,#13811,.T.);
#18023=ORIENTED_EDGE('',*,*,#13812,.T.);
#18024=ORIENTED_EDGE('',*,*,#13813,.T.);
#18025=ORIENTED_EDGE('',*,*,#13814,.T.);
#18026=ORIENTED_EDGE('',*,*,#13815,.T.);
#18027=ORIENTED_EDGE('',*,*,#13816,.T.);
#18028=ORIENTED_EDGE('',*,*,#13817,.T.);
#18029=ORIENTED_EDGE('',*,*,#13818,.T.);
#18030=ORIENTED_EDGE('',*,*,#13819,.F.);
#18031=ORIENTED_EDGE('',*,*,#13820,.T.);
#18032=ORIENTED_EDGE('',*,*,#13821,.T.);
#18033=ORIENTED_EDGE('',*,*,#13822,.F.);
#18034=ORIENTED_EDGE('',*,*,#13823,.T.);
#18035=ORIENTED_EDGE('',*,*,#13824,.T.);
#18036=ORIENTED_EDGE('',*,*,#13825,.T.);
#18037=ORIENTED_EDGE('',*,*,#13826,.T.);
#18038=ORIENTED_EDGE('',*,*,#13827,.T.);
#18039=ORIENTED_EDGE('',*,*,#13828,.T.);
#18040=ORIENTED_EDGE('',*,*,#13829,.T.);
#18041=ORIENTED_EDGE('',*,*,#13830,.T.);
#18042=ORIENTED_EDGE('',*,*,#13831,.T.);
#18043=ORIENTED_EDGE('',*,*,#13832,.T.);
#18044=ORIENTED_EDGE('',*,*,#13833,.T.);
#18045=ORIENTED_EDGE('',*,*,#13834,.T.);
#18046=ORIENTED_EDGE('',*,*,#13835,.T.);
#18047=ORIENTED_EDGE('',*,*,#13836,.T.);
#18048=ORIENTED_EDGE('',*,*,#13837,.T.);
#18049=ORIENTED_EDGE('',*,*,#13838,.T.);
#18050=ORIENTED_EDGE('',*,*,#13839,.F.);
#18051=ORIENTED_EDGE('',*,*,#13840,.T.);
#18052=ORIENTED_EDGE('',*,*,#13841,.T.);
#18053=ORIENTED_EDGE('',*,*,#13842,.F.);
#18054=ORIENTED_EDGE('',*,*,#13843,.T.);
#18055=ORIENTED_EDGE('',*,*,#13844,.T.);
#18056=ORIENTED_EDGE('',*,*,#13845,.T.);
#18057=ORIENTED_EDGE('',*,*,#13846,.T.);
#18058=ORIENTED_EDGE('',*,*,#13847,.T.);
#18059=ORIENTED_EDGE('',*,*,#13848,.T.);
#18060=ORIENTED_EDGE('',*,*,#13849,.T.);
#18061=ORIENTED_EDGE('',*,*,#13850,.T.);
#18062=ORIENTED_EDGE('',*,*,#13851,.T.);
#18063=ORIENTED_EDGE('',*,*,#13852,.T.);
#18064=ORIENTED_EDGE('',*,*,#13853,.T.);
#18065=ORIENTED_EDGE('',*,*,#13854,.T.);
#18066=ORIENTED_EDGE('',*,*,#13855,.T.);
#18067=ORIENTED_EDGE('',*,*,#13856,.T.);
#18068=ORIENTED_EDGE('',*,*,#13857,.T.);
#18069=ORIENTED_EDGE('',*,*,#13858,.T.);
#18070=ORIENTED_EDGE('',*,*,#13859,.F.);
#18071=ORIENTED_EDGE('',*,*,#13860,.T.);
#18072=ORIENTED_EDGE('',*,*,#13861,.T.);
#18073=ORIENTED_EDGE('',*,*,#13862,.F.);
#18074=ORIENTED_EDGE('',*,*,#13863,.T.);
#18075=ORIENTED_EDGE('',*,*,#13864,.T.);
#18076=ORIENTED_EDGE('',*,*,#13865,.T.);
#18077=ORIENTED_EDGE('',*,*,#13866,.T.);
#18078=ORIENTED_EDGE('',*,*,#13867,.T.);
#18079=ORIENTED_EDGE('',*,*,#13868,.T.);
#18080=ORIENTED_EDGE('',*,*,#13869,.T.);
#18081=ORIENTED_EDGE('',*,*,#13870,.T.);
#18082=ORIENTED_EDGE('',*,*,#13871,.T.);
#18083=ORIENTED_EDGE('',*,*,#13872,.T.);
#18084=ORIENTED_EDGE('',*,*,#13873,.T.);
#18085=ORIENTED_EDGE('',*,*,#13874,.T.);
#18086=ORIENTED_EDGE('',*,*,#13875,.T.);
#18087=ORIENTED_EDGE('',*,*,#13876,.T.);
#18088=ORIENTED_EDGE('',*,*,#13877,.T.);
#18089=ORIENTED_EDGE('',*,*,#13878,.T.);
#18090=ORIENTED_EDGE('',*,*,#13879,.F.);
#18091=ORIENTED_EDGE('',*,*,#13880,.T.);
#18092=ORIENTED_EDGE('',*,*,#13881,.T.);
#18093=ORIENTED_EDGE('',*,*,#13882,.F.);
#18094=ORIENTED_EDGE('',*,*,#13883,.T.);
#18095=ORIENTED_EDGE('',*,*,#13884,.T.);
#18096=ORIENTED_EDGE('',*,*,#13885,.T.);
#18097=ORIENTED_EDGE('',*,*,#13886,.T.);
#18098=ORIENTED_EDGE('',*,*,#13887,.T.);
#18099=ORIENTED_EDGE('',*,*,#13888,.T.);
#18100=ORIENTED_EDGE('',*,*,#13889,.T.);
#18101=ORIENTED_EDGE('',*,*,#13890,.T.);
#18102=ORIENTED_EDGE('',*,*,#13891,.T.);
#18103=ORIENTED_EDGE('',*,*,#13892,.T.);
#18104=ORIENTED_EDGE('',*,*,#13893,.T.);
#18105=ORIENTED_EDGE('',*,*,#13894,.T.);
#18106=ORIENTED_EDGE('',*,*,#13895,.T.);
#18107=ORIENTED_EDGE('',*,*,#13896,.T.);
#18108=ORIENTED_EDGE('',*,*,#13897,.T.);
#18109=ORIENTED_EDGE('',*,*,#13898,.T.);
#18110=ORIENTED_EDGE('',*,*,#13899,.F.);
#18111=ORIENTED_EDGE('',*,*,#13900,.T.);
#18112=ORIENTED_EDGE('',*,*,#13901,.T.);
#18113=ORIENTED_EDGE('',*,*,#13902,.F.);
#18114=ORIENTED_EDGE('',*,*,#13903,.T.);
#18115=ORIENTED_EDGE('',*,*,#13904,.T.);
#18116=ORIENTED_EDGE('',*,*,#13905,.T.);
#18117=ORIENTED_EDGE('',*,*,#13906,.T.);
#18118=ORIENTED_EDGE('',*,*,#13907,.T.);
#18119=ORIENTED_EDGE('',*,*,#13908,.T.);
#18120=ORIENTED_EDGE('',*,*,#13909,.T.);
#18121=ORIENTED_EDGE('',*,*,#13910,.T.);
#18122=ORIENTED_EDGE('',*,*,#13911,.T.);
#18123=ORIENTED_EDGE('',*,*,#13912,.T.);
#18124=ORIENTED_EDGE('',*,*,#13913,.T.);
#18125=ORIENTED_EDGE('',*,*,#13914,.T.);
#18126=ORIENTED_EDGE('',*,*,#13915,.T.);
#18127=ORIENTED_EDGE('',*,*,#13916,.T.);
#18128=ORIENTED_EDGE('',*,*,#13917,.T.);
#18129=ORIENTED_EDGE('',*,*,#13918,.T.);
#18130=ORIENTED_EDGE('',*,*,#13919,.F.);
#18131=ORIENTED_EDGE('',*,*,#13920,.T.);
#18132=ORIENTED_EDGE('',*,*,#13921,.T.);
#18133=ORIENTED_EDGE('',*,*,#13922,.F.);
#18134=ORIENTED_EDGE('',*,*,#13923,.T.);
#18135=ORIENTED_EDGE('',*,*,#13924,.T.);
#18136=ORIENTED_EDGE('',*,*,#13925,.T.);
#18137=ORIENTED_EDGE('',*,*,#13926,.T.);
#18138=ORIENTED_EDGE('',*,*,#13927,.T.);
#18139=ORIENTED_EDGE('',*,*,#13928,.T.);
#18140=ORIENTED_EDGE('',*,*,#13929,.T.);
#18141=ORIENTED_EDGE('',*,*,#13930,.T.);
#18142=ORIENTED_EDGE('',*,*,#13931,.T.);
#18143=ORIENTED_EDGE('',*,*,#13932,.T.);
#18144=ORIENTED_EDGE('',*,*,#13933,.T.);
#18145=ORIENTED_EDGE('',*,*,#13934,.T.);
#18146=ORIENTED_EDGE('',*,*,#13935,.T.);
#18147=ORIENTED_EDGE('',*,*,#13936,.T.);
#18148=ORIENTED_EDGE('',*,*,#13937,.T.);
#18149=ORIENTED_EDGE('',*,*,#13938,.T.);
#18150=ORIENTED_EDGE('',*,*,#13939,.F.);
#18151=ORIENTED_EDGE('',*,*,#13940,.T.);
#18152=ORIENTED_EDGE('',*,*,#13941,.T.);
#18153=ORIENTED_EDGE('',*,*,#13942,.F.);
#18154=ORIENTED_EDGE('',*,*,#13943,.T.);
#18155=ORIENTED_EDGE('',*,*,#13944,.T.);
#18156=ORIENTED_EDGE('',*,*,#13945,.T.);
#18157=ORIENTED_EDGE('',*,*,#13946,.T.);
#18158=ORIENTED_EDGE('',*,*,#13947,.T.);
#18159=ORIENTED_EDGE('',*,*,#13948,.T.);
#18160=ORIENTED_EDGE('',*,*,#13949,.T.);
#18161=ORIENTED_EDGE('',*,*,#13950,.T.);
#18162=ORIENTED_EDGE('',*,*,#13951,.T.);
#18163=ORIENTED_EDGE('',*,*,#13952,.T.);
#18164=ORIENTED_EDGE('',*,*,#13953,.T.);
#18165=ORIENTED_EDGE('',*,*,#13954,.T.);
#18166=ORIENTED_EDGE('',*,*,#13955,.T.);
#18167=ORIENTED_EDGE('',*,*,#13956,.T.);
#18168=ORIENTED_EDGE('',*,*,#13957,.T.);
#18169=ORIENTED_EDGE('',*,*,#13958,.T.);
#18170=ORIENTED_EDGE('',*,*,#13959,.F.);
#18171=ORIENTED_EDGE('',*,*,#13960,.T.);
#18172=ORIENTED_EDGE('',*,*,#13961,.F.);
#18173=ORIENTED_EDGE('',*,*,#13716,.F.);
#18174=ORIENTED_EDGE('',*,*,#13962,.T.);
#18175=ORIENTED_EDGE('',*,*,#13963,.F.);
#18176=ORIENTED_EDGE('',*,*,#13964,.F.);
#18177=ORIENTED_EDGE('',*,*,#13965,.F.);
#18178=ORIENTED_EDGE('',*,*,#13723,.F.);
#18179=ORIENTED_EDGE('',*,*,#13721,.F.);
#18180=ORIENTED_EDGE('',*,*,#13966,.T.);
#18181=ORIENTED_EDGE('',*,*,#13967,.F.);
#18182=ORIENTED_EDGE('',*,*,#13962,.F.);
#18183=ORIENTED_EDGE('',*,*,#13968,.T.);
#18184=ORIENTED_EDGE('',*,*,#13942,.T.);
#18185=ORIENTED_EDGE('',*,*,#13969,.T.);
#18186=ORIENTED_EDGE('',*,*,#13970,.T.);
#18187=ORIENTED_EDGE('',*,*,#13971,.T.);
#18188=ORIENTED_EDGE('',*,*,#13972,.T.);
#18189=ORIENTED_EDGE('',*,*,#13968,.F.);
#18190=ORIENTED_EDGE('',*,*,#13973,.T.);
#18191=ORIENTED_EDGE('',*,*,#13974,.F.);
#18192=ORIENTED_EDGE('',*,*,#13975,.F.);
#18193=ORIENTED_EDGE('',*,*,#13976,.F.);
#18194=ORIENTED_EDGE('',*,*,#13943,.F.);
#18195=ORIENTED_EDGE('',*,*,#13972,.F.);
#18196=ORIENTED_EDGE('',*,*,#13977,.T.);
#18197=ORIENTED_EDGE('',*,*,#13978,.F.);
#18198=ORIENTED_EDGE('',*,*,#13973,.F.);
#18199=ORIENTED_EDGE('',*,*,#13979,.T.);
#18200=ORIENTED_EDGE('',*,*,#13922,.T.);
#18201=ORIENTED_EDGE('',*,*,#13980,.T.);
#18202=ORIENTED_EDGE('',*,*,#13981,.T.);
#18203=ORIENTED_EDGE('',*,*,#13982,.T.);
#18204=ORIENTED_EDGE('',*,*,#13983,.T.);
#18205=ORIENTED_EDGE('',*,*,#13979,.F.);
#18206=ORIENTED_EDGE('',*,*,#13984,.T.);
#18207=ORIENTED_EDGE('',*,*,#13985,.F.);
#18208=ORIENTED_EDGE('',*,*,#13986,.F.);
#18209=ORIENTED_EDGE('',*,*,#13987,.F.);
#18210=ORIENTED_EDGE('',*,*,#13923,.F.);
#18211=ORIENTED_EDGE('',*,*,#13983,.F.);
#18212=ORIENTED_EDGE('',*,*,#13988,.T.);
#18213=ORIENTED_EDGE('',*,*,#13989,.F.);
#18214=ORIENTED_EDGE('',*,*,#13984,.F.);
#18215=ORIENTED_EDGE('',*,*,#13990,.T.);
#18216=ORIENTED_EDGE('',*,*,#13902,.T.);
#18217=ORIENTED_EDGE('',*,*,#13991,.T.);
#18218=ORIENTED_EDGE('',*,*,#13992,.T.);
#18219=ORIENTED_EDGE('',*,*,#13993,.T.);
#18220=ORIENTED_EDGE('',*,*,#13994,.T.);
#18221=ORIENTED_EDGE('',*,*,#13990,.F.);
#18222=ORIENTED_EDGE('',*,*,#13995,.T.);
#18223=ORIENTED_EDGE('',*,*,#13996,.F.);
#18224=ORIENTED_EDGE('',*,*,#13997,.F.);
#18225=ORIENTED_EDGE('',*,*,#13998,.F.);
#18226=ORIENTED_EDGE('',*,*,#13903,.F.);
#18227=ORIENTED_EDGE('',*,*,#13994,.F.);
#18228=ORIENTED_EDGE('',*,*,#13999,.T.);
#18229=ORIENTED_EDGE('',*,*,#14000,.F.);
#18230=ORIENTED_EDGE('',*,*,#13995,.F.);
#18231=ORIENTED_EDGE('',*,*,#14001,.T.);
#18232=ORIENTED_EDGE('',*,*,#13882,.T.);
#18233=ORIENTED_EDGE('',*,*,#14002,.T.);
#18234=ORIENTED_EDGE('',*,*,#14003,.T.);
#18235=ORIENTED_EDGE('',*,*,#14004,.T.);
#18236=ORIENTED_EDGE('',*,*,#14005,.T.);
#18237=ORIENTED_EDGE('',*,*,#14001,.F.);
#18238=ORIENTED_EDGE('',*,*,#14006,.T.);
#18239=ORIENTED_EDGE('',*,*,#14007,.F.);
#18240=ORIENTED_EDGE('',*,*,#14008,.F.);
#18241=ORIENTED_EDGE('',*,*,#14009,.F.);
#18242=ORIENTED_EDGE('',*,*,#13883,.F.);
#18243=ORIENTED_EDGE('',*,*,#14005,.F.);
#18244=ORIENTED_EDGE('',*,*,#14010,.T.);
#18245=ORIENTED_EDGE('',*,*,#14011,.F.);
#18246=ORIENTED_EDGE('',*,*,#14006,.F.);
#18247=ORIENTED_EDGE('',*,*,#14012,.T.);
#18248=ORIENTED_EDGE('',*,*,#13862,.T.);
#18249=ORIENTED_EDGE('',*,*,#14013,.T.);
#18250=ORIENTED_EDGE('',*,*,#14014,.T.);
#18251=ORIENTED_EDGE('',*,*,#14015,.T.);
#18252=ORIENTED_EDGE('',*,*,#14016,.T.);
#18253=ORIENTED_EDGE('',*,*,#14012,.F.);
#18254=ORIENTED_EDGE('',*,*,#14017,.T.);
#18255=ORIENTED_EDGE('',*,*,#14018,.F.);
#18256=ORIENTED_EDGE('',*,*,#14019,.F.);
#18257=ORIENTED_EDGE('',*,*,#14020,.F.);
#18258=ORIENTED_EDGE('',*,*,#13863,.F.);
#18259=ORIENTED_EDGE('',*,*,#14016,.F.);
#18260=ORIENTED_EDGE('',*,*,#14021,.T.);
#18261=ORIENTED_EDGE('',*,*,#14022,.F.);
#18262=ORIENTED_EDGE('',*,*,#14017,.F.);
#18263=ORIENTED_EDGE('',*,*,#14023,.T.);
#18264=ORIENTED_EDGE('',*,*,#13842,.T.);
#18265=ORIENTED_EDGE('',*,*,#14024,.T.);
#18266=ORIENTED_EDGE('',*,*,#14025,.T.);
#18267=ORIENTED_EDGE('',*,*,#14026,.T.);
#18268=ORIENTED_EDGE('',*,*,#14027,.T.);
#18269=ORIENTED_EDGE('',*,*,#14023,.F.);
#18270=ORIENTED_EDGE('',*,*,#14028,.T.);
#18271=ORIENTED_EDGE('',*,*,#14029,.F.);
#18272=ORIENTED_EDGE('',*,*,#14030,.F.);
#18273=ORIENTED_EDGE('',*,*,#14031,.F.);
#18274=ORIENTED_EDGE('',*,*,#13843,.F.);
#18275=ORIENTED_EDGE('',*,*,#14027,.F.);
#18276=ORIENTED_EDGE('',*,*,#14032,.T.);
#18277=ORIENTED_EDGE('',*,*,#14033,.F.);
#18278=ORIENTED_EDGE('',*,*,#14028,.F.);
#18279=ORIENTED_EDGE('',*,*,#14034,.T.);
#18280=ORIENTED_EDGE('',*,*,#13822,.T.);
#18281=ORIENTED_EDGE('',*,*,#14035,.T.);
#18282=ORIENTED_EDGE('',*,*,#14036,.T.);
#18283=ORIENTED_EDGE('',*,*,#14037,.T.);
#18284=ORIENTED_EDGE('',*,*,#14038,.T.);
#18285=ORIENTED_EDGE('',*,*,#14034,.F.);
#18286=ORIENTED_EDGE('',*,*,#14039,.T.);
#18287=ORIENTED_EDGE('',*,*,#14040,.F.);
#18288=ORIENTED_EDGE('',*,*,#14041,.F.);
#18289=ORIENTED_EDGE('',*,*,#14042,.F.);
#18290=ORIENTED_EDGE('',*,*,#13823,.F.);
#18291=ORIENTED_EDGE('',*,*,#14038,.F.);
#18292=ORIENTED_EDGE('',*,*,#14043,.T.);
#18293=ORIENTED_EDGE('',*,*,#14044,.F.);
#18294=ORIENTED_EDGE('',*,*,#14039,.F.);
#18295=ORIENTED_EDGE('',*,*,#14045,.T.);
#18296=ORIENTED_EDGE('',*,*,#13802,.T.);
#18297=ORIENTED_EDGE('',*,*,#14046,.T.);
#18298=ORIENTED_EDGE('',*,*,#14047,.T.);
#18299=ORIENTED_EDGE('',*,*,#14048,.T.);
#18300=ORIENTED_EDGE('',*,*,#14049,.T.);
#18301=ORIENTED_EDGE('',*,*,#14045,.F.);
#18302=ORIENTED_EDGE('',*,*,#14050,.T.);
#18303=ORIENTED_EDGE('',*,*,#14051,.F.);
#18304=ORIENTED_EDGE('',*,*,#14052,.F.);
#18305=ORIENTED_EDGE('',*,*,#14053,.F.);
#18306=ORIENTED_EDGE('',*,*,#13803,.F.);
#18307=ORIENTED_EDGE('',*,*,#14049,.F.);
#18308=ORIENTED_EDGE('',*,*,#14054,.T.);
#18309=ORIENTED_EDGE('',*,*,#14055,.F.);
#18310=ORIENTED_EDGE('',*,*,#14050,.F.);
#18311=ORIENTED_EDGE('',*,*,#14056,.T.);
#18312=ORIENTED_EDGE('',*,*,#13782,.T.);
#18313=ORIENTED_EDGE('',*,*,#14057,.T.);
#18314=ORIENTED_EDGE('',*,*,#14058,.T.);
#18315=ORIENTED_EDGE('',*,*,#14059,.T.);
#18316=ORIENTED_EDGE('',*,*,#14060,.T.);
#18317=ORIENTED_EDGE('',*,*,#14056,.F.);
#18318=ORIENTED_EDGE('',*,*,#14061,.T.);
#18319=ORIENTED_EDGE('',*,*,#14062,.F.);
#18320=ORIENTED_EDGE('',*,*,#14063,.F.);
#18321=ORIENTED_EDGE('',*,*,#14064,.F.);
#18322=ORIENTED_EDGE('',*,*,#13783,.F.);
#18323=ORIENTED_EDGE('',*,*,#14060,.F.);
#18324=ORIENTED_EDGE('',*,*,#14065,.T.);
#18325=ORIENTED_EDGE('',*,*,#14066,.F.);
#18326=ORIENTED_EDGE('',*,*,#14061,.F.);
#18327=ORIENTED_EDGE('',*,*,#14067,.T.);
#18328=ORIENTED_EDGE('',*,*,#13762,.T.);
#18329=ORIENTED_EDGE('',*,*,#14068,.T.);
#18330=ORIENTED_EDGE('',*,*,#14069,.T.);
#18331=ORIENTED_EDGE('',*,*,#14070,.T.);
#18332=ORIENTED_EDGE('',*,*,#14071,.T.);
#18333=ORIENTED_EDGE('',*,*,#14067,.F.);
#18334=ORIENTED_EDGE('',*,*,#14072,.T.);
#18335=ORIENTED_EDGE('',*,*,#14073,.F.);
#18336=ORIENTED_EDGE('',*,*,#14074,.F.);
#18337=ORIENTED_EDGE('',*,*,#14075,.F.);
#18338=ORIENTED_EDGE('',*,*,#13763,.F.);
#18339=ORIENTED_EDGE('',*,*,#14071,.F.);
#18340=ORIENTED_EDGE('',*,*,#14076,.T.);
#18341=ORIENTED_EDGE('',*,*,#14077,.F.);
#18342=ORIENTED_EDGE('',*,*,#14072,.F.);
#18343=ORIENTED_EDGE('',*,*,#14078,.T.);
#18344=ORIENTED_EDGE('',*,*,#13742,.T.);
#18345=ORIENTED_EDGE('',*,*,#14079,.T.);
#18346=ORIENTED_EDGE('',*,*,#14080,.T.);
#18347=ORIENTED_EDGE('',*,*,#14081,.T.);
#18348=ORIENTED_EDGE('',*,*,#14082,.T.);
#18349=ORIENTED_EDGE('',*,*,#14078,.F.);
#18350=ORIENTED_EDGE('',*,*,#14083,.T.);
#18351=ORIENTED_EDGE('',*,*,#14084,.F.);
#18352=ORIENTED_EDGE('',*,*,#14085,.F.);
#18353=ORIENTED_EDGE('',*,*,#14086,.F.);
#18354=ORIENTED_EDGE('',*,*,#13743,.F.);
#18355=ORIENTED_EDGE('',*,*,#14082,.F.);
#18356=ORIENTED_EDGE('',*,*,#14087,.T.);
#18357=ORIENTED_EDGE('',*,*,#14088,.F.);
#18358=ORIENTED_EDGE('',*,*,#14083,.F.);
#18359=ORIENTED_EDGE('',*,*,#14089,.T.);
#18360=ORIENTED_EDGE('',*,*,#14090,.T.);
#18361=ORIENTED_EDGE('',*,*,#14091,.T.);
#18362=ORIENTED_EDGE('',*,*,#13739,.T.);
#18363=ORIENTED_EDGE('',*,*,#14092,.T.);
#18364=ORIENTED_EDGE('',*,*,#14093,.T.);
#18365=ORIENTED_EDGE('',*,*,#14090,.F.);
#18366=ORIENTED_EDGE('',*,*,#14094,.T.);
#18367=ORIENTED_EDGE('',*,*,#14095,.F.);
#18368=ORIENTED_EDGE('',*,*,#14096,.F.);
#18369=ORIENTED_EDGE('',*,*,#14089,.F.);
#18370=ORIENTED_EDGE('',*,*,#14097,.T.);
#18371=ORIENTED_EDGE('',*,*,#14098,.F.);
#18372=ORIENTED_EDGE('',*,*,#14094,.F.);
#18373=ORIENTED_EDGE('',*,*,#14099,.T.);
#18374=ORIENTED_EDGE('',*,*,#14100,.T.);
#18375=ORIENTED_EDGE('',*,*,#14101,.T.);
#18376=ORIENTED_EDGE('',*,*,#13959,.T.);
#18377=ORIENTED_EDGE('',*,*,#14102,.T.);
#18378=ORIENTED_EDGE('',*,*,#14103,.T.);
#18379=ORIENTED_EDGE('',*,*,#14100,.F.);
#18380=ORIENTED_EDGE('',*,*,#14104,.T.);
#18381=ORIENTED_EDGE('',*,*,#14105,.F.);
#18382=ORIENTED_EDGE('',*,*,#14106,.F.);
#18383=ORIENTED_EDGE('',*,*,#14099,.F.);
#18384=ORIENTED_EDGE('',*,*,#14107,.T.);
#18385=ORIENTED_EDGE('',*,*,#14108,.F.);
#18386=ORIENTED_EDGE('',*,*,#14104,.F.);
#18387=ORIENTED_EDGE('',*,*,#14109,.T.);
#18388=ORIENTED_EDGE('',*,*,#14110,.T.);
#18389=ORIENTED_EDGE('',*,*,#14111,.T.);
#18390=ORIENTED_EDGE('',*,*,#13939,.T.);
#18391=ORIENTED_EDGE('',*,*,#14112,.T.);
#18392=ORIENTED_EDGE('',*,*,#14113,.T.);
#18393=ORIENTED_EDGE('',*,*,#14110,.F.);
#18394=ORIENTED_EDGE('',*,*,#14114,.T.);
#18395=ORIENTED_EDGE('',*,*,#14115,.F.);
#18396=ORIENTED_EDGE('',*,*,#14116,.F.);
#18397=ORIENTED_EDGE('',*,*,#14109,.F.);
#18398=ORIENTED_EDGE('',*,*,#14117,.T.);
#18399=ORIENTED_EDGE('',*,*,#14118,.F.);
#18400=ORIENTED_EDGE('',*,*,#14114,.F.);
#18401=ORIENTED_EDGE('',*,*,#14119,.T.);
#18402=ORIENTED_EDGE('',*,*,#14120,.T.);
#18403=ORIENTED_EDGE('',*,*,#14121,.T.);
#18404=ORIENTED_EDGE('',*,*,#13919,.T.);
#18405=ORIENTED_EDGE('',*,*,#14122,.T.);
#18406=ORIENTED_EDGE('',*,*,#14123,.T.);
#18407=ORIENTED_EDGE('',*,*,#14120,.F.);
#18408=ORIENTED_EDGE('',*,*,#14124,.T.);
#18409=ORIENTED_EDGE('',*,*,#14125,.F.);
#18410=ORIENTED_EDGE('',*,*,#14126,.F.);
#18411=ORIENTED_EDGE('',*,*,#14119,.F.);
#18412=ORIENTED_EDGE('',*,*,#14127,.T.);
#18413=ORIENTED_EDGE('',*,*,#14128,.F.);
#18414=ORIENTED_EDGE('',*,*,#14124,.F.);
#18415=ORIENTED_EDGE('',*,*,#14129,.T.);
#18416=ORIENTED_EDGE('',*,*,#14130,.T.);
#18417=ORIENTED_EDGE('',*,*,#14131,.T.);
#18418=ORIENTED_EDGE('',*,*,#13899,.T.);
#18419=ORIENTED_EDGE('',*,*,#14132,.T.);
#18420=ORIENTED_EDGE('',*,*,#14133,.T.);
#18421=ORIENTED_EDGE('',*,*,#14130,.F.);
#18422=ORIENTED_EDGE('',*,*,#14134,.T.);
#18423=ORIENTED_EDGE('',*,*,#14135,.F.);
#18424=ORIENTED_EDGE('',*,*,#14136,.F.);
#18425=ORIENTED_EDGE('',*,*,#14129,.F.);
#18426=ORIENTED_EDGE('',*,*,#14137,.T.);
#18427=ORIENTED_EDGE('',*,*,#14138,.F.);
#18428=ORIENTED_EDGE('',*,*,#14134,.F.);
#18429=ORIENTED_EDGE('',*,*,#14139,.T.);
#18430=ORIENTED_EDGE('',*,*,#14140,.T.);
#18431=ORIENTED_EDGE('',*,*,#14141,.T.);
#18432=ORIENTED_EDGE('',*,*,#13879,.T.);
#18433=ORIENTED_EDGE('',*,*,#14142,.T.);
#18434=ORIENTED_EDGE('',*,*,#14143,.T.);
#18435=ORIENTED_EDGE('',*,*,#14140,.F.);
#18436=ORIENTED_EDGE('',*,*,#14144,.T.);
#18437=ORIENTED_EDGE('',*,*,#14145,.F.);
#18438=ORIENTED_EDGE('',*,*,#14146,.F.);
#18439=ORIENTED_EDGE('',*,*,#14139,.F.);
#18440=ORIENTED_EDGE('',*,*,#14147,.T.);
#18441=ORIENTED_EDGE('',*,*,#14148,.F.);
#18442=ORIENTED_EDGE('',*,*,#14144,.F.);
#18443=ORIENTED_EDGE('',*,*,#14149,.T.);
#18444=ORIENTED_EDGE('',*,*,#14150,.T.);
#18445=ORIENTED_EDGE('',*,*,#14151,.T.);
#18446=ORIENTED_EDGE('',*,*,#13859,.T.);
#18447=ORIENTED_EDGE('',*,*,#14152,.T.);
#18448=ORIENTED_EDGE('',*,*,#14153,.T.);
#18449=ORIENTED_EDGE('',*,*,#14150,.F.);
#18450=ORIENTED_EDGE('',*,*,#14154,.T.);
#18451=ORIENTED_EDGE('',*,*,#14155,.F.);
#18452=ORIENTED_EDGE('',*,*,#14156,.F.);
#18453=ORIENTED_EDGE('',*,*,#14149,.F.);
#18454=ORIENTED_EDGE('',*,*,#14157,.T.);
#18455=ORIENTED_EDGE('',*,*,#14158,.F.);
#18456=ORIENTED_EDGE('',*,*,#14154,.F.);
#18457=ORIENTED_EDGE('',*,*,#14159,.T.);
#18458=ORIENTED_EDGE('',*,*,#14160,.T.);
#18459=ORIENTED_EDGE('',*,*,#14161,.T.);
#18460=ORIENTED_EDGE('',*,*,#13839,.T.);
#18461=ORIENTED_EDGE('',*,*,#14162,.T.);
#18462=ORIENTED_EDGE('',*,*,#14163,.T.);
#18463=ORIENTED_EDGE('',*,*,#14160,.F.);
#18464=ORIENTED_EDGE('',*,*,#14164,.T.);
#18465=ORIENTED_EDGE('',*,*,#14165,.F.);
#18466=ORIENTED_EDGE('',*,*,#14166,.F.);
#18467=ORIENTED_EDGE('',*,*,#14159,.F.);
#18468=ORIENTED_EDGE('',*,*,#14167,.T.);
#18469=ORIENTED_EDGE('',*,*,#14168,.F.);
#18470=ORIENTED_EDGE('',*,*,#14164,.F.);
#18471=ORIENTED_EDGE('',*,*,#14169,.T.);
#18472=ORIENTED_EDGE('',*,*,#14170,.T.);
#18473=ORIENTED_EDGE('',*,*,#14171,.T.);
#18474=ORIENTED_EDGE('',*,*,#13819,.T.);
#18475=ORIENTED_EDGE('',*,*,#14172,.T.);
#18476=ORIENTED_EDGE('',*,*,#14173,.T.);
#18477=ORIENTED_EDGE('',*,*,#14170,.F.);
#18478=ORIENTED_EDGE('',*,*,#14174,.T.);
#18479=ORIENTED_EDGE('',*,*,#14175,.F.);
#18480=ORIENTED_EDGE('',*,*,#14176,.F.);
#18481=ORIENTED_EDGE('',*,*,#14169,.F.);
#18482=ORIENTED_EDGE('',*,*,#14177,.T.);
#18483=ORIENTED_EDGE('',*,*,#14178,.F.);
#18484=ORIENTED_EDGE('',*,*,#14174,.F.);
#18485=ORIENTED_EDGE('',*,*,#14179,.T.);
#18486=ORIENTED_EDGE('',*,*,#14180,.T.);
#18487=ORIENTED_EDGE('',*,*,#14181,.T.);
#18488=ORIENTED_EDGE('',*,*,#13799,.T.);
#18489=ORIENTED_EDGE('',*,*,#14182,.T.);
#18490=ORIENTED_EDGE('',*,*,#14183,.T.);
#18491=ORIENTED_EDGE('',*,*,#14180,.F.);
#18492=ORIENTED_EDGE('',*,*,#14184,.T.);
#18493=ORIENTED_EDGE('',*,*,#14185,.F.);
#18494=ORIENTED_EDGE('',*,*,#14186,.F.);
#18495=ORIENTED_EDGE('',*,*,#14179,.F.);
#18496=ORIENTED_EDGE('',*,*,#14187,.T.);
#18497=ORIENTED_EDGE('',*,*,#14188,.F.);
#18498=ORIENTED_EDGE('',*,*,#14184,.F.);
#18499=ORIENTED_EDGE('',*,*,#14189,.T.);
#18500=ORIENTED_EDGE('',*,*,#14190,.T.);
#18501=ORIENTED_EDGE('',*,*,#14191,.T.);
#18502=ORIENTED_EDGE('',*,*,#13779,.T.);
#18503=ORIENTED_EDGE('',*,*,#14192,.T.);
#18504=ORIENTED_EDGE('',*,*,#14193,.T.);
#18505=ORIENTED_EDGE('',*,*,#14190,.F.);
#18506=ORIENTED_EDGE('',*,*,#14194,.T.);
#18507=ORIENTED_EDGE('',*,*,#14195,.F.);
#18508=ORIENTED_EDGE('',*,*,#14196,.F.);
#18509=ORIENTED_EDGE('',*,*,#14189,.F.);
#18510=ORIENTED_EDGE('',*,*,#14197,.T.);
#18511=ORIENTED_EDGE('',*,*,#14198,.F.);
#18512=ORIENTED_EDGE('',*,*,#14194,.F.);
#18513=ORIENTED_EDGE('',*,*,#14199,.T.);
#18514=ORIENTED_EDGE('',*,*,#14200,.T.);
#18515=ORIENTED_EDGE('',*,*,#14201,.T.);
#18516=ORIENTED_EDGE('',*,*,#13759,.T.);
#18517=ORIENTED_EDGE('',*,*,#14202,.T.);
#18518=ORIENTED_EDGE('',*,*,#14203,.T.);
#18519=ORIENTED_EDGE('',*,*,#14200,.F.);
#18520=ORIENTED_EDGE('',*,*,#14204,.T.);
#18521=ORIENTED_EDGE('',*,*,#14205,.F.);
#18522=ORIENTED_EDGE('',*,*,#14206,.F.);
#18523=ORIENTED_EDGE('',*,*,#14199,.F.);
#18524=ORIENTED_EDGE('',*,*,#14207,.T.);
#18525=ORIENTED_EDGE('',*,*,#14208,.F.);
#18526=ORIENTED_EDGE('',*,*,#14204,.F.);
#18527=ORIENTED_EDGE('',*,*,#14209,.T.);
#18528=ORIENTED_EDGE('',*,*,#14210,.T.);
#18529=ORIENTED_EDGE('',*,*,#14211,.T.);
#18530=ORIENTED_EDGE('',*,*,#14212,.T.);
#18531=ORIENTED_EDGE('',*,*,#14084,.T.);
#18532=ORIENTED_EDGE('',*,*,#14088,.T.);
#18533=ORIENTED_EDGE('',*,*,#14212,.F.);
#18534=ORIENTED_EDGE('',*,*,#14213,.T.);
#18535=ORIENTED_EDGE('',*,*,#14214,.T.);
#18536=ORIENTED_EDGE('',*,*,#14215,.F.);
#18537=ORIENTED_EDGE('',*,*,#14216,.T.);
#18538=ORIENTED_EDGE('',*,*,#14217,.T.);
#18539=ORIENTED_EDGE('',*,*,#14218,.T.);
#18540=ORIENTED_EDGE('',*,*,#14219,.T.);
#18541=ORIENTED_EDGE('',*,*,#14220,.T.);
#18542=ORIENTED_EDGE('',*,*,#14221,.T.);
#18543=ORIENTED_EDGE('',*,*,#14222,.T.);
#18544=ORIENTED_EDGE('',*,*,#14223,.T.);
#18545=ORIENTED_EDGE('',*,*,#14224,.T.);
#18546=ORIENTED_EDGE('',*,*,#14225,.T.);
#18547=ORIENTED_EDGE('',*,*,#14226,.T.);
#18548=ORIENTED_EDGE('',*,*,#14227,.T.);
#18549=ORIENTED_EDGE('',*,*,#14228,.T.);
#18550=ORIENTED_EDGE('',*,*,#14229,.T.);
#18551=ORIENTED_EDGE('',*,*,#14230,.T.);
#18552=ORIENTED_EDGE('',*,*,#13964,.T.);
#18553=ORIENTED_EDGE('',*,*,#14231,.F.);
#18554=ORIENTED_EDGE('',*,*,#14232,.T.);
#18555=ORIENTED_EDGE('',*,*,#14233,.T.);
#18556=ORIENTED_EDGE('',*,*,#14234,.F.);
#18557=ORIENTED_EDGE('',*,*,#14235,.T.);
#18558=ORIENTED_EDGE('',*,*,#14236,.T.);
#18559=ORIENTED_EDGE('',*,*,#14237,.T.);
#18560=ORIENTED_EDGE('',*,*,#14238,.T.);
#18561=ORIENTED_EDGE('',*,*,#14239,.T.);
#18562=ORIENTED_EDGE('',*,*,#14240,.T.);
#18563=ORIENTED_EDGE('',*,*,#14241,.T.);
#18564=ORIENTED_EDGE('',*,*,#14242,.T.);
#18565=ORIENTED_EDGE('',*,*,#14243,.T.);
#18566=ORIENTED_EDGE('',*,*,#14244,.T.);
#18567=ORIENTED_EDGE('',*,*,#14245,.T.);
#18568=ORIENTED_EDGE('',*,*,#14246,.T.);
#18569=ORIENTED_EDGE('',*,*,#14247,.T.);
#18570=ORIENTED_EDGE('',*,*,#14248,.T.);
#18571=ORIENTED_EDGE('',*,*,#14249,.T.);
#18572=ORIENTED_EDGE('',*,*,#13975,.T.);
#18573=ORIENTED_EDGE('',*,*,#14250,.F.);
#18574=ORIENTED_EDGE('',*,*,#14251,.T.);
#18575=ORIENTED_EDGE('',*,*,#14252,.T.);
#18576=ORIENTED_EDGE('',*,*,#14253,.F.);
#18577=ORIENTED_EDGE('',*,*,#14254,.T.);
#18578=ORIENTED_EDGE('',*,*,#14255,.T.);
#18579=ORIENTED_EDGE('',*,*,#14256,.T.);
#18580=ORIENTED_EDGE('',*,*,#14257,.T.);
#18581=ORIENTED_EDGE('',*,*,#14258,.T.);
#18582=ORIENTED_EDGE('',*,*,#14259,.T.);
#18583=ORIENTED_EDGE('',*,*,#14260,.T.);
#18584=ORIENTED_EDGE('',*,*,#14261,.T.);
#18585=ORIENTED_EDGE('',*,*,#14262,.T.);
#18586=ORIENTED_EDGE('',*,*,#14263,.T.);
#18587=ORIENTED_EDGE('',*,*,#14264,.T.);
#18588=ORIENTED_EDGE('',*,*,#14265,.T.);
#18589=ORIENTED_EDGE('',*,*,#14266,.T.);
#18590=ORIENTED_EDGE('',*,*,#14267,.T.);
#18591=ORIENTED_EDGE('',*,*,#14268,.T.);
#18592=ORIENTED_EDGE('',*,*,#13986,.T.);
#18593=ORIENTED_EDGE('',*,*,#14269,.F.);
#18594=ORIENTED_EDGE('',*,*,#14270,.T.);
#18595=ORIENTED_EDGE('',*,*,#14271,.T.);
#18596=ORIENTED_EDGE('',*,*,#14272,.F.);
#18597=ORIENTED_EDGE('',*,*,#14273,.T.);
#18598=ORIENTED_EDGE('',*,*,#14274,.T.);
#18599=ORIENTED_EDGE('',*,*,#14275,.T.);
#18600=ORIENTED_EDGE('',*,*,#14276,.T.);
#18601=ORIENTED_EDGE('',*,*,#14277,.T.);
#18602=ORIENTED_EDGE('',*,*,#14278,.T.);
#18603=ORIENTED_EDGE('',*,*,#14279,.T.);
#18604=ORIENTED_EDGE('',*,*,#14280,.T.);
#18605=ORIENTED_EDGE('',*,*,#14281,.T.);
#18606=ORIENTED_EDGE('',*,*,#14282,.T.);
#18607=ORIENTED_EDGE('',*,*,#14283,.T.);
#18608=ORIENTED_EDGE('',*,*,#14284,.T.);
#18609=ORIENTED_EDGE('',*,*,#14285,.T.);
#18610=ORIENTED_EDGE('',*,*,#14286,.T.);
#18611=ORIENTED_EDGE('',*,*,#14287,.T.);
#18612=ORIENTED_EDGE('',*,*,#13997,.T.);
#18613=ORIENTED_EDGE('',*,*,#14288,.F.);
#18614=ORIENTED_EDGE('',*,*,#14289,.T.);
#18615=ORIENTED_EDGE('',*,*,#14290,.T.);
#18616=ORIENTED_EDGE('',*,*,#14291,.F.);
#18617=ORIENTED_EDGE('',*,*,#14292,.T.);
#18618=ORIENTED_EDGE('',*,*,#14293,.T.);
#18619=ORIENTED_EDGE('',*,*,#14294,.T.);
#18620=ORIENTED_EDGE('',*,*,#14295,.T.);
#18621=ORIENTED_EDGE('',*,*,#14296,.T.);
#18622=ORIENTED_EDGE('',*,*,#14297,.T.);
#18623=ORIENTED_EDGE('',*,*,#14298,.T.);
#18624=ORIENTED_EDGE('',*,*,#14299,.T.);
#18625=ORIENTED_EDGE('',*,*,#14300,.T.);
#18626=ORIENTED_EDGE('',*,*,#14301,.T.);
#18627=ORIENTED_EDGE('',*,*,#14302,.T.);
#18628=ORIENTED_EDGE('',*,*,#14303,.T.);
#18629=ORIENTED_EDGE('',*,*,#14304,.T.);
#18630=ORIENTED_EDGE('',*,*,#14305,.T.);
#18631=ORIENTED_EDGE('',*,*,#14306,.T.);
#18632=ORIENTED_EDGE('',*,*,#14008,.T.);
#18633=ORIENTED_EDGE('',*,*,#14307,.F.);
#18634=ORIENTED_EDGE('',*,*,#14308,.T.);
#18635=ORIENTED_EDGE('',*,*,#14309,.T.);
#18636=ORIENTED_EDGE('',*,*,#14310,.F.);
#18637=ORIENTED_EDGE('',*,*,#14311,.T.);
#18638=ORIENTED_EDGE('',*,*,#14312,.T.);
#18639=ORIENTED_EDGE('',*,*,#14313,.T.);
#18640=ORIENTED_EDGE('',*,*,#14314,.T.);
#18641=ORIENTED_EDGE('',*,*,#14315,.T.);
#18642=ORIENTED_EDGE('',*,*,#14316,.T.);
#18643=ORIENTED_EDGE('',*,*,#14317,.T.);
#18644=ORIENTED_EDGE('',*,*,#14318,.T.);
#18645=ORIENTED_EDGE('',*,*,#14319,.T.);
#18646=ORIENTED_EDGE('',*,*,#14320,.T.);
#18647=ORIENTED_EDGE('',*,*,#14321,.T.);
#18648=ORIENTED_EDGE('',*,*,#14322,.T.);
#18649=ORIENTED_EDGE('',*,*,#14323,.T.);
#18650=ORIENTED_EDGE('',*,*,#14324,.T.);
#18651=ORIENTED_EDGE('',*,*,#14325,.T.);
#18652=ORIENTED_EDGE('',*,*,#14019,.T.);
#18653=ORIENTED_EDGE('',*,*,#14326,.F.);
#18654=ORIENTED_EDGE('',*,*,#14327,.T.);
#18655=ORIENTED_EDGE('',*,*,#14328,.T.);
#18656=ORIENTED_EDGE('',*,*,#14329,.F.);
#18657=ORIENTED_EDGE('',*,*,#14330,.T.);
#18658=ORIENTED_EDGE('',*,*,#14331,.T.);
#18659=ORIENTED_EDGE('',*,*,#14332,.T.);
#18660=ORIENTED_EDGE('',*,*,#14333,.T.);
#18661=ORIENTED_EDGE('',*,*,#14334,.T.);
#18662=ORIENTED_EDGE('',*,*,#14335,.T.);
#18663=ORIENTED_EDGE('',*,*,#14336,.T.);
#18664=ORIENTED_EDGE('',*,*,#14337,.T.);
#18665=ORIENTED_EDGE('',*,*,#14338,.T.);
#18666=ORIENTED_EDGE('',*,*,#14339,.T.);
#18667=ORIENTED_EDGE('',*,*,#14340,.T.);
#18668=ORIENTED_EDGE('',*,*,#14341,.T.);
#18669=ORIENTED_EDGE('',*,*,#14342,.T.);
#18670=ORIENTED_EDGE('',*,*,#14343,.T.);
#18671=ORIENTED_EDGE('',*,*,#14344,.T.);
#18672=ORIENTED_EDGE('',*,*,#14030,.T.);
#18673=ORIENTED_EDGE('',*,*,#14345,.F.);
#18674=ORIENTED_EDGE('',*,*,#14346,.T.);
#18675=ORIENTED_EDGE('',*,*,#14347,.T.);
#18676=ORIENTED_EDGE('',*,*,#14348,.F.);
#18677=ORIENTED_EDGE('',*,*,#14349,.T.);
#18678=ORIENTED_EDGE('',*,*,#14350,.T.);
#18679=ORIENTED_EDGE('',*,*,#14351,.T.);
#18680=ORIENTED_EDGE('',*,*,#14352,.T.);
#18681=ORIENTED_EDGE('',*,*,#14353,.T.);
#18682=ORIENTED_EDGE('',*,*,#14354,.T.);
#18683=ORIENTED_EDGE('',*,*,#14355,.T.);
#18684=ORIENTED_EDGE('',*,*,#14356,.T.);
#18685=ORIENTED_EDGE('',*,*,#14357,.T.);
#18686=ORIENTED_EDGE('',*,*,#14358,.T.);
#18687=ORIENTED_EDGE('',*,*,#14359,.T.);
#18688=ORIENTED_EDGE('',*,*,#14360,.T.);
#18689=ORIENTED_EDGE('',*,*,#14361,.T.);
#18690=ORIENTED_EDGE('',*,*,#14362,.T.);
#18691=ORIENTED_EDGE('',*,*,#14363,.T.);
#18692=ORIENTED_EDGE('',*,*,#14041,.T.);
#18693=ORIENTED_EDGE('',*,*,#14364,.F.);
#18694=ORIENTED_EDGE('',*,*,#14365,.T.);
#18695=ORIENTED_EDGE('',*,*,#14366,.T.);
#18696=ORIENTED_EDGE('',*,*,#14367,.F.);
#18697=ORIENTED_EDGE('',*,*,#14368,.T.);
#18698=ORIENTED_EDGE('',*,*,#14369,.T.);
#18699=ORIENTED_EDGE('',*,*,#14370,.T.);
#18700=ORIENTED_EDGE('',*,*,#14371,.T.);
#18701=ORIENTED_EDGE('',*,*,#14372,.T.);
#18702=ORIENTED_EDGE('',*,*,#14373,.T.);
#18703=ORIENTED_EDGE('',*,*,#14374,.T.);
#18704=ORIENTED_EDGE('',*,*,#14375,.T.);
#18705=ORIENTED_EDGE('',*,*,#14376,.T.);
#18706=ORIENTED_EDGE('',*,*,#14377,.T.);
#18707=ORIENTED_EDGE('',*,*,#14378,.T.);
#18708=ORIENTED_EDGE('',*,*,#14379,.T.);
#18709=ORIENTED_EDGE('',*,*,#14380,.T.);
#18710=ORIENTED_EDGE('',*,*,#14381,.T.);
#18711=ORIENTED_EDGE('',*,*,#14382,.T.);
#18712=ORIENTED_EDGE('',*,*,#14052,.T.);
#18713=ORIENTED_EDGE('',*,*,#14383,.F.);
#18714=ORIENTED_EDGE('',*,*,#14384,.T.);
#18715=ORIENTED_EDGE('',*,*,#14385,.T.);
#18716=ORIENTED_EDGE('',*,*,#14386,.F.);
#18717=ORIENTED_EDGE('',*,*,#14387,.T.);
#18718=ORIENTED_EDGE('',*,*,#14388,.T.);
#18719=ORIENTED_EDGE('',*,*,#14389,.T.);
#18720=ORIENTED_EDGE('',*,*,#14390,.T.);
#18721=ORIENTED_EDGE('',*,*,#14391,.T.);
#18722=ORIENTED_EDGE('',*,*,#14392,.T.);
#18723=ORIENTED_EDGE('',*,*,#14393,.T.);
#18724=ORIENTED_EDGE('',*,*,#14394,.T.);
#18725=ORIENTED_EDGE('',*,*,#14395,.T.);
#18726=ORIENTED_EDGE('',*,*,#14396,.T.);
#18727=ORIENTED_EDGE('',*,*,#14397,.T.);
#18728=ORIENTED_EDGE('',*,*,#14398,.T.);
#18729=ORIENTED_EDGE('',*,*,#14399,.T.);
#18730=ORIENTED_EDGE('',*,*,#14400,.T.);
#18731=ORIENTED_EDGE('',*,*,#14401,.T.);
#18732=ORIENTED_EDGE('',*,*,#14063,.T.);
#18733=ORIENTED_EDGE('',*,*,#14402,.F.);
#18734=ORIENTED_EDGE('',*,*,#14403,.T.);
#18735=ORIENTED_EDGE('',*,*,#14404,.T.);
#18736=ORIENTED_EDGE('',*,*,#14405,.F.);
#18737=ORIENTED_EDGE('',*,*,#14406,.T.);
#18738=ORIENTED_EDGE('',*,*,#14407,.T.);
#18739=ORIENTED_EDGE('',*,*,#14408,.T.);
#18740=ORIENTED_EDGE('',*,*,#14409,.T.);
#18741=ORIENTED_EDGE('',*,*,#14410,.T.);
#18742=ORIENTED_EDGE('',*,*,#14411,.T.);
#18743=ORIENTED_EDGE('',*,*,#14412,.T.);
#18744=ORIENTED_EDGE('',*,*,#14413,.T.);
#18745=ORIENTED_EDGE('',*,*,#14414,.T.);
#18746=ORIENTED_EDGE('',*,*,#14415,.T.);
#18747=ORIENTED_EDGE('',*,*,#14416,.T.);
#18748=ORIENTED_EDGE('',*,*,#14417,.T.);
#18749=ORIENTED_EDGE('',*,*,#14418,.T.);
#18750=ORIENTED_EDGE('',*,*,#14419,.T.);
#18751=ORIENTED_EDGE('',*,*,#14420,.T.);
#18752=ORIENTED_EDGE('',*,*,#14074,.T.);
#18753=ORIENTED_EDGE('',*,*,#14421,.F.);
#18754=ORIENTED_EDGE('',*,*,#14422,.T.);
#18755=ORIENTED_EDGE('',*,*,#14423,.T.);
#18756=ORIENTED_EDGE('',*,*,#14424,.F.);
#18757=ORIENTED_EDGE('',*,*,#14425,.T.);
#18758=ORIENTED_EDGE('',*,*,#14426,.T.);
#18759=ORIENTED_EDGE('',*,*,#14427,.T.);
#18760=ORIENTED_EDGE('',*,*,#14428,.T.);
#18761=ORIENTED_EDGE('',*,*,#14429,.T.);
#18762=ORIENTED_EDGE('',*,*,#14430,.T.);
#18763=ORIENTED_EDGE('',*,*,#14431,.T.);
#18764=ORIENTED_EDGE('',*,*,#14432,.T.);
#18765=ORIENTED_EDGE('',*,*,#14433,.T.);
#18766=ORIENTED_EDGE('',*,*,#14434,.T.);
#18767=ORIENTED_EDGE('',*,*,#14435,.T.);
#18768=ORIENTED_EDGE('',*,*,#14436,.T.);
#18769=ORIENTED_EDGE('',*,*,#14437,.T.);
#18770=ORIENTED_EDGE('',*,*,#14438,.T.);
#18771=ORIENTED_EDGE('',*,*,#14439,.T.);
#18772=ORIENTED_EDGE('',*,*,#14085,.T.);
#18773=ORIENTED_EDGE('',*,*,#14440,.F.);
#18774=ORIENTED_EDGE('',*,*,#14441,.T.);
#18775=ORIENTED_EDGE('',*,*,#14424,.T.);
#18776=ORIENTED_EDGE('',*,*,#14442,.T.);
#18777=ORIENTED_EDGE('',*,*,#14205,.T.);
#18778=ORIENTED_EDGE('',*,*,#14208,.T.);
#18779=ORIENTED_EDGE('',*,*,#14443,.T.);
#18780=ORIENTED_EDGE('',*,*,#14444,.T.);
#18781=ORIENTED_EDGE('',*,*,#14445,.T.);
#18782=ORIENTED_EDGE('',*,*,#14446,.T.);
#18783=ORIENTED_EDGE('',*,*,#14421,.T.);
#18784=ORIENTED_EDGE('',*,*,#14073,.T.);
#18785=ORIENTED_EDGE('',*,*,#14077,.T.);
#18786=ORIENTED_EDGE('',*,*,#14447,.T.);
#18787=ORIENTED_EDGE('',*,*,#14405,.T.);
#18788=ORIENTED_EDGE('',*,*,#14448,.T.);
#18789=ORIENTED_EDGE('',*,*,#14195,.T.);
#18790=ORIENTED_EDGE('',*,*,#14198,.T.);
#18791=ORIENTED_EDGE('',*,*,#14449,.T.);
#18792=ORIENTED_EDGE('',*,*,#14450,.T.);
#18793=ORIENTED_EDGE('',*,*,#14451,.T.);
#18794=ORIENTED_EDGE('',*,*,#14452,.T.);
#18795=ORIENTED_EDGE('',*,*,#14402,.T.);
#18796=ORIENTED_EDGE('',*,*,#14062,.T.);
#18797=ORIENTED_EDGE('',*,*,#14066,.T.);
#18798=ORIENTED_EDGE('',*,*,#14453,.T.);
#18799=ORIENTED_EDGE('',*,*,#14386,.T.);
#18800=ORIENTED_EDGE('',*,*,#14454,.T.);
#18801=ORIENTED_EDGE('',*,*,#14185,.T.);
#18802=ORIENTED_EDGE('',*,*,#14188,.T.);
#18803=ORIENTED_EDGE('',*,*,#14455,.T.);
#18804=ORIENTED_EDGE('',*,*,#14456,.T.);
#18805=ORIENTED_EDGE('',*,*,#14457,.T.);
#18806=ORIENTED_EDGE('',*,*,#14458,.T.);
#18807=ORIENTED_EDGE('',*,*,#14383,.T.);
#18808=ORIENTED_EDGE('',*,*,#14051,.T.);
#18809=ORIENTED_EDGE('',*,*,#14055,.T.);
#18810=ORIENTED_EDGE('',*,*,#14459,.T.);
#18811=ORIENTED_EDGE('',*,*,#14367,.T.);
#18812=ORIENTED_EDGE('',*,*,#14460,.T.);
#18813=ORIENTED_EDGE('',*,*,#14175,.T.);
#18814=ORIENTED_EDGE('',*,*,#14178,.T.);
#18815=ORIENTED_EDGE('',*,*,#14461,.T.);
#18816=ORIENTED_EDGE('',*,*,#14462,.T.);
#18817=ORIENTED_EDGE('',*,*,#14463,.T.);
#18818=ORIENTED_EDGE('',*,*,#14464,.T.);
#18819=ORIENTED_EDGE('',*,*,#14364,.T.);
#18820=ORIENTED_EDGE('',*,*,#14040,.T.);
#18821=ORIENTED_EDGE('',*,*,#14044,.T.);
#18822=ORIENTED_EDGE('',*,*,#14465,.T.);
#18823=ORIENTED_EDGE('',*,*,#14348,.T.);
#18824=ORIENTED_EDGE('',*,*,#14466,.T.);
#18825=ORIENTED_EDGE('',*,*,#14165,.T.);
#18826=ORIENTED_EDGE('',*,*,#14168,.T.);
#18827=ORIENTED_EDGE('',*,*,#14467,.T.);
#18828=ORIENTED_EDGE('',*,*,#14468,.T.);
#18829=ORIENTED_EDGE('',*,*,#14469,.T.);
#18830=ORIENTED_EDGE('',*,*,#14470,.T.);
#18831=ORIENTED_EDGE('',*,*,#14345,.T.);
#18832=ORIENTED_EDGE('',*,*,#14029,.T.);
#18833=ORIENTED_EDGE('',*,*,#14033,.T.);
#18834=ORIENTED_EDGE('',*,*,#14471,.T.);
#18835=ORIENTED_EDGE('',*,*,#14329,.T.);
#18836=ORIENTED_EDGE('',*,*,#14472,.T.);
#18837=ORIENTED_EDGE('',*,*,#14155,.T.);
#18838=ORIENTED_EDGE('',*,*,#14158,.T.);
#18839=ORIENTED_EDGE('',*,*,#14473,.T.);
#18840=ORIENTED_EDGE('',*,*,#14474,.T.);
#18841=ORIENTED_EDGE('',*,*,#14475,.T.);
#18842=ORIENTED_EDGE('',*,*,#14476,.T.);
#18843=ORIENTED_EDGE('',*,*,#14326,.T.);
#18844=ORIENTED_EDGE('',*,*,#14018,.T.);
#18845=ORIENTED_EDGE('',*,*,#14022,.T.);
#18846=ORIENTED_EDGE('',*,*,#14477,.T.);
#18847=ORIENTED_EDGE('',*,*,#14310,.T.);
#18848=ORIENTED_EDGE('',*,*,#14478,.T.);
#18849=ORIENTED_EDGE('',*,*,#14145,.T.);
#18850=ORIENTED_EDGE('',*,*,#14148,.T.);
#18851=ORIENTED_EDGE('',*,*,#14479,.T.);
#18852=ORIENTED_EDGE('',*,*,#14480,.T.);
#18853=ORIENTED_EDGE('',*,*,#14481,.T.);
#18854=ORIENTED_EDGE('',*,*,#14482,.T.);
#18855=ORIENTED_EDGE('',*,*,#14307,.T.);
#18856=ORIENTED_EDGE('',*,*,#14007,.T.);
#18857=ORIENTED_EDGE('',*,*,#14011,.T.);
#18858=ORIENTED_EDGE('',*,*,#14483,.T.);
#18859=ORIENTED_EDGE('',*,*,#14291,.T.);
#18860=ORIENTED_EDGE('',*,*,#14484,.T.);
#18861=ORIENTED_EDGE('',*,*,#14135,.T.);
#18862=ORIENTED_EDGE('',*,*,#14138,.T.);
#18863=ORIENTED_EDGE('',*,*,#14485,.T.);
#18864=ORIENTED_EDGE('',*,*,#14486,.T.);
#18865=ORIENTED_EDGE('',*,*,#14487,.T.);
#18866=ORIENTED_EDGE('',*,*,#14488,.T.);
#18867=ORIENTED_EDGE('',*,*,#14288,.T.);
#18868=ORIENTED_EDGE('',*,*,#13996,.T.);
#18869=ORIENTED_EDGE('',*,*,#14000,.T.);
#18870=ORIENTED_EDGE('',*,*,#14489,.T.);
#18871=ORIENTED_EDGE('',*,*,#14272,.T.);
#18872=ORIENTED_EDGE('',*,*,#14490,.T.);
#18873=ORIENTED_EDGE('',*,*,#14125,.T.);
#18874=ORIENTED_EDGE('',*,*,#14128,.T.);
#18875=ORIENTED_EDGE('',*,*,#14491,.T.);
#18876=ORIENTED_EDGE('',*,*,#14492,.T.);
#18877=ORIENTED_EDGE('',*,*,#14493,.T.);
#18878=ORIENTED_EDGE('',*,*,#14494,.T.);
#18879=ORIENTED_EDGE('',*,*,#14269,.T.);
#18880=ORIENTED_EDGE('',*,*,#13985,.T.);
#18881=ORIENTED_EDGE('',*,*,#13989,.T.);
#18882=ORIENTED_EDGE('',*,*,#14495,.T.);
#18883=ORIENTED_EDGE('',*,*,#14253,.T.);
#18884=ORIENTED_EDGE('',*,*,#14496,.T.);
#18885=ORIENTED_EDGE('',*,*,#14115,.T.);
#18886=ORIENTED_EDGE('',*,*,#14118,.T.);
#18887=ORIENTED_EDGE('',*,*,#14497,.T.);
#18888=ORIENTED_EDGE('',*,*,#14498,.T.);
#18889=ORIENTED_EDGE('',*,*,#14499,.T.);
#18890=ORIENTED_EDGE('',*,*,#14500,.T.);
#18891=ORIENTED_EDGE('',*,*,#14250,.T.);
#18892=ORIENTED_EDGE('',*,*,#13974,.T.);
#18893=ORIENTED_EDGE('',*,*,#13978,.T.);
#18894=ORIENTED_EDGE('',*,*,#14501,.T.);
#18895=ORIENTED_EDGE('',*,*,#14234,.T.);
#18896=ORIENTED_EDGE('',*,*,#14502,.T.);
#18897=ORIENTED_EDGE('',*,*,#14105,.T.);
#18898=ORIENTED_EDGE('',*,*,#14108,.T.);
#18899=ORIENTED_EDGE('',*,*,#14503,.T.);
#18900=ORIENTED_EDGE('',*,*,#14504,.T.);
#18901=ORIENTED_EDGE('',*,*,#14505,.T.);
#18902=ORIENTED_EDGE('',*,*,#14506,.T.);
#18903=ORIENTED_EDGE('',*,*,#14231,.T.);
#18904=ORIENTED_EDGE('',*,*,#13963,.T.);
#18905=ORIENTED_EDGE('',*,*,#13967,.T.);
#18906=ORIENTED_EDGE('',*,*,#14507,.T.);
#18907=ORIENTED_EDGE('',*,*,#14215,.T.);
#18908=ORIENTED_EDGE('',*,*,#14508,.T.);
#18909=ORIENTED_EDGE('',*,*,#14095,.T.);
#18910=ORIENTED_EDGE('',*,*,#14098,.T.);
#18911=ORIENTED_EDGE('',*,*,#14509,.T.);
#18912=ORIENTED_EDGE('',*,*,#14510,.F.);
#18913=ORIENTED_EDGE('',*,*,#14511,.T.);
#18914=ORIENTED_EDGE('',*,*,#14512,.T.);
#18915=ORIENTED_EDGE('',*,*,#14513,.F.);
#18916=ORIENTED_EDGE('',*,*,#14514,.F.);
#18917=ORIENTED_EDGE('',*,*,#14513,.T.);
#18918=ORIENTED_EDGE('',*,*,#14515,.T.);
#18919=ORIENTED_EDGE('',*,*,#14516,.F.);
#18920=ORIENTED_EDGE('',*,*,#14517,.F.);
#18921=ORIENTED_EDGE('',*,*,#14518,.T.);
#18922=ORIENTED_EDGE('',*,*,#14519,.T.);
#18923=ORIENTED_EDGE('',*,*,#14511,.F.);
#18924=ORIENTED_EDGE('',*,*,#14520,.F.);
#18925=ORIENTED_EDGE('',*,*,#14516,.T.);
#18926=ORIENTED_EDGE('',*,*,#14521,.T.);
#18927=ORIENTED_EDGE('',*,*,#14518,.F.);
#18928=ORIENTED_EDGE('',*,*,#14515,.F.);
#18929=ORIENTED_EDGE('',*,*,#14512,.F.);
#18930=ORIENTED_EDGE('',*,*,#14519,.F.);
#18931=ORIENTED_EDGE('',*,*,#14521,.F.);
#18932=ORIENTED_EDGE('',*,*,#13741,.F.);
#18933=ORIENTED_EDGE('',*,*,#14522,.T.);
#18934=ORIENTED_EDGE('',*,*,#14213,.F.);
#18935=ORIENTED_EDGE('',*,*,#14211,.F.);
#18936=ORIENTED_EDGE('',*,*,#14523,.F.);
#18937=ORIENTED_EDGE('',*,*,#14079,.F.);
#18938=ORIENTED_EDGE('',*,*,#14080,.F.);
#18939=ORIENTED_EDGE('',*,*,#14523,.T.);
#18940=ORIENTED_EDGE('',*,*,#14210,.F.);
#18941=ORIENTED_EDGE('',*,*,#14524,.F.);
#18942=ORIENTED_EDGE('',*,*,#14081,.F.);
#18943=ORIENTED_EDGE('',*,*,#14524,.T.);
#18944=ORIENTED_EDGE('',*,*,#14209,.F.);
#18945=ORIENTED_EDGE('',*,*,#14087,.F.);
#18946=ORIENTED_EDGE('',*,*,#13744,.F.);
#18947=ORIENTED_EDGE('',*,*,#14086,.T.);
#18948=ORIENTED_EDGE('',*,*,#14439,.F.);
#18949=ORIENTED_EDGE('',*,*,#14525,.F.);
#18950=ORIENTED_EDGE('',*,*,#13745,.F.);
#18951=ORIENTED_EDGE('',*,*,#14525,.T.);
#18952=ORIENTED_EDGE('',*,*,#14438,.F.);
#18953=ORIENTED_EDGE('',*,*,#14526,.F.);
#18954=ORIENTED_EDGE('',*,*,#13746,.F.);
#18955=ORIENTED_EDGE('',*,*,#14526,.T.);
#18956=ORIENTED_EDGE('',*,*,#14437,.F.);
#18957=ORIENTED_EDGE('',*,*,#14527,.F.);
#18958=ORIENTED_EDGE('',*,*,#13747,.F.);
#18959=ORIENTED_EDGE('',*,*,#14527,.T.);
#18960=ORIENTED_EDGE('',*,*,#14436,.F.);
#18961=ORIENTED_EDGE('',*,*,#14528,.F.);
#18962=ORIENTED_EDGE('',*,*,#13748,.F.);
#18963=ORIENTED_EDGE('',*,*,#14528,.T.);
#18964=ORIENTED_EDGE('',*,*,#14435,.F.);
#18965=ORIENTED_EDGE('',*,*,#14529,.F.);
#18966=ORIENTED_EDGE('',*,*,#13749,.F.);
#18967=ORIENTED_EDGE('',*,*,#14529,.T.);
#18968=ORIENTED_EDGE('',*,*,#14434,.F.);
#18969=ORIENTED_EDGE('',*,*,#14530,.F.);
#18970=ORIENTED_EDGE('',*,*,#13750,.F.);
#18971=ORIENTED_EDGE('',*,*,#14530,.T.);
#18972=ORIENTED_EDGE('',*,*,#14433,.F.);
#18973=ORIENTED_EDGE('',*,*,#14531,.F.);
#18974=ORIENTED_EDGE('',*,*,#13751,.F.);
#18975=ORIENTED_EDGE('',*,*,#14531,.T.);
#18976=ORIENTED_EDGE('',*,*,#14432,.F.);
#18977=ORIENTED_EDGE('',*,*,#14532,.F.);
#18978=ORIENTED_EDGE('',*,*,#13752,.F.);
#18979=ORIENTED_EDGE('',*,*,#14532,.T.);
#18980=ORIENTED_EDGE('',*,*,#14431,.F.);
#18981=ORIENTED_EDGE('',*,*,#14533,.F.);
#18982=ORIENTED_EDGE('',*,*,#13753,.F.);
#18983=ORIENTED_EDGE('',*,*,#14533,.T.);
#18984=ORIENTED_EDGE('',*,*,#14430,.F.);
#18985=ORIENTED_EDGE('',*,*,#14534,.F.);
#18986=ORIENTED_EDGE('',*,*,#13754,.F.);
#18987=ORIENTED_EDGE('',*,*,#14534,.T.);
#18988=ORIENTED_EDGE('',*,*,#14429,.F.);
#18989=ORIENTED_EDGE('',*,*,#14535,.F.);
#18990=ORIENTED_EDGE('',*,*,#13755,.F.);
#18991=ORIENTED_EDGE('',*,*,#14535,.T.);
#18992=ORIENTED_EDGE('',*,*,#14428,.F.);
#18993=ORIENTED_EDGE('',*,*,#14536,.F.);
#18994=ORIENTED_EDGE('',*,*,#13756,.F.);
#18995=ORIENTED_EDGE('',*,*,#14536,.T.);
#18996=ORIENTED_EDGE('',*,*,#14427,.F.);
#18997=ORIENTED_EDGE('',*,*,#14537,.F.);
#18998=ORIENTED_EDGE('',*,*,#13757,.F.);
#18999=ORIENTED_EDGE('',*,*,#14537,.T.);
#19000=ORIENTED_EDGE('',*,*,#14426,.F.);
#19001=ORIENTED_EDGE('',*,*,#14538,.F.);
#19002=ORIENTED_EDGE('',*,*,#14202,.F.);
#19003=ORIENTED_EDGE('',*,*,#13758,.F.);
#19004=ORIENTED_EDGE('',*,*,#14538,.T.);
#19005=ORIENTED_EDGE('',*,*,#14425,.F.);
#19006=ORIENTED_EDGE('',*,*,#14441,.F.);
#19007=ORIENTED_EDGE('',*,*,#14539,.F.);
#19008=ORIENTED_EDGE('',*,*,#14203,.F.);
#19009=ORIENTED_EDGE('',*,*,#14539,.T.);
#19010=ORIENTED_EDGE('',*,*,#14443,.F.);
#19011=ORIENTED_EDGE('',*,*,#14207,.F.);
#19012=ORIENTED_EDGE('',*,*,#13760,.F.);
#19013=ORIENTED_EDGE('',*,*,#14201,.F.);
#19014=ORIENTED_EDGE('',*,*,#14206,.T.);
#19015=ORIENTED_EDGE('',*,*,#14442,.F.);
#19016=ORIENTED_EDGE('',*,*,#14423,.F.);
#19017=ORIENTED_EDGE('',*,*,#14540,.F.);
#19018=ORIENTED_EDGE('',*,*,#13761,.F.);
#19019=ORIENTED_EDGE('',*,*,#14540,.T.);
#19020=ORIENTED_EDGE('',*,*,#14422,.F.);
#19021=ORIENTED_EDGE('',*,*,#14446,.F.);
#19022=ORIENTED_EDGE('',*,*,#14541,.F.);
#19023=ORIENTED_EDGE('',*,*,#14068,.F.);
#19024=ORIENTED_EDGE('',*,*,#14069,.F.);
#19025=ORIENTED_EDGE('',*,*,#14541,.T.);
#19026=ORIENTED_EDGE('',*,*,#14445,.F.);
#19027=ORIENTED_EDGE('',*,*,#14542,.F.);
#19028=ORIENTED_EDGE('',*,*,#14070,.F.);
#19029=ORIENTED_EDGE('',*,*,#14542,.T.);
#19030=ORIENTED_EDGE('',*,*,#14444,.F.);
#19031=ORIENTED_EDGE('',*,*,#14076,.F.);
#19032=ORIENTED_EDGE('',*,*,#13764,.F.);
#19033=ORIENTED_EDGE('',*,*,#14075,.T.);
#19034=ORIENTED_EDGE('',*,*,#14420,.F.);
#19035=ORIENTED_EDGE('',*,*,#14543,.F.);
#19036=ORIENTED_EDGE('',*,*,#13765,.F.);
#19037=ORIENTED_EDGE('',*,*,#14543,.T.);
#19038=ORIENTED_EDGE('',*,*,#14419,.F.);
#19039=ORIENTED_EDGE('',*,*,#14544,.F.);
#19040=ORIENTED_EDGE('',*,*,#13766,.F.);
#19041=ORIENTED_EDGE('',*,*,#14544,.T.);
#19042=ORIENTED_EDGE('',*,*,#14418,.F.);
#19043=ORIENTED_EDGE('',*,*,#14545,.F.);
#19044=ORIENTED_EDGE('',*,*,#13767,.F.);
#19045=ORIENTED_EDGE('',*,*,#14545,.T.);
#19046=ORIENTED_EDGE('',*,*,#14417,.F.);
#19047=ORIENTED_EDGE('',*,*,#14546,.F.);
#19048=ORIENTED_EDGE('',*,*,#13768,.F.);
#19049=ORIENTED_EDGE('',*,*,#14546,.T.);
#19050=ORIENTED_EDGE('',*,*,#14416,.F.);
#19051=ORIENTED_EDGE('',*,*,#14547,.F.);
#19052=ORIENTED_EDGE('',*,*,#13769,.F.);
#19053=ORIENTED_EDGE('',*,*,#14547,.T.);
#19054=ORIENTED_EDGE('',*,*,#14415,.F.);
#19055=ORIENTED_EDGE('',*,*,#14548,.F.);
#19056=ORIENTED_EDGE('',*,*,#13770,.F.);
#19057=ORIENTED_EDGE('',*,*,#14548,.T.);
#19058=ORIENTED_EDGE('',*,*,#14414,.F.);
#19059=ORIENTED_EDGE('',*,*,#14549,.F.);
#19060=ORIENTED_EDGE('',*,*,#13771,.F.);
#19061=ORIENTED_EDGE('',*,*,#14549,.T.);
#19062=ORIENTED_EDGE('',*,*,#14413,.F.);
#19063=ORIENTED_EDGE('',*,*,#14550,.F.);
#19064=ORIENTED_EDGE('',*,*,#13772,.F.);
#19065=ORIENTED_EDGE('',*,*,#14550,.T.);
#19066=ORIENTED_EDGE('',*,*,#14412,.F.);
#19067=ORIENTED_EDGE('',*,*,#14551,.F.);
#19068=ORIENTED_EDGE('',*,*,#13773,.F.);
#19069=ORIENTED_EDGE('',*,*,#14551,.T.);
#19070=ORIENTED_EDGE('',*,*,#14411,.F.);
#19071=ORIENTED_EDGE('',*,*,#14552,.F.);
#19072=ORIENTED_EDGE('',*,*,#13774,.F.);
#19073=ORIENTED_EDGE('',*,*,#14552,.T.);
#19074=ORIENTED_EDGE('',*,*,#14410,.F.);
#19075=ORIENTED_EDGE('',*,*,#14553,.F.);
#19076=ORIENTED_EDGE('',*,*,#13775,.F.);
#19077=ORIENTED_EDGE('',*,*,#14553,.T.);
#19078=ORIENTED_EDGE('',*,*,#14409,.F.);
#19079=ORIENTED_EDGE('',*,*,#14554,.F.);
#19080=ORIENTED_EDGE('',*,*,#13776,.F.);
#19081=ORIENTED_EDGE('',*,*,#14554,.T.);
#19082=ORIENTED_EDGE('',*,*,#14408,.F.);
#19083=ORIENTED_EDGE('',*,*,#14555,.F.);
#19084=ORIENTED_EDGE('',*,*,#13777,.F.);
#19085=ORIENTED_EDGE('',*,*,#14555,.T.);
#19086=ORIENTED_EDGE('',*,*,#14407,.F.);
#19087=ORIENTED_EDGE('',*,*,#14556,.F.);
#19088=ORIENTED_EDGE('',*,*,#14192,.F.);
#19089=ORIENTED_EDGE('',*,*,#13778,.F.);
#19090=ORIENTED_EDGE('',*,*,#14556,.T.);
#19091=ORIENTED_EDGE('',*,*,#14406,.F.);
#19092=ORIENTED_EDGE('',*,*,#14447,.F.);
#19093=ORIENTED_EDGE('',*,*,#14557,.F.);
#19094=ORIENTED_EDGE('',*,*,#14193,.F.);
#19095=ORIENTED_EDGE('',*,*,#14557,.T.);
#19096=ORIENTED_EDGE('',*,*,#14449,.F.);
#19097=ORIENTED_EDGE('',*,*,#14197,.F.);
#19098=ORIENTED_EDGE('',*,*,#13780,.F.);
#19099=ORIENTED_EDGE('',*,*,#14191,.F.);
#19100=ORIENTED_EDGE('',*,*,#14196,.T.);
#19101=ORIENTED_EDGE('',*,*,#14448,.F.);
#19102=ORIENTED_EDGE('',*,*,#14404,.F.);
#19103=ORIENTED_EDGE('',*,*,#14558,.F.);
#19104=ORIENTED_EDGE('',*,*,#13781,.F.);
#19105=ORIENTED_EDGE('',*,*,#14558,.T.);
#19106=ORIENTED_EDGE('',*,*,#14403,.F.);
#19107=ORIENTED_EDGE('',*,*,#14452,.F.);
#19108=ORIENTED_EDGE('',*,*,#14559,.F.);
#19109=ORIENTED_EDGE('',*,*,#14057,.F.);
#19110=ORIENTED_EDGE('',*,*,#14058,.F.);
#19111=ORIENTED_EDGE('',*,*,#14559,.T.);
#19112=ORIENTED_EDGE('',*,*,#14451,.F.);
#19113=ORIENTED_EDGE('',*,*,#14560,.F.);
#19114=ORIENTED_EDGE('',*,*,#14059,.F.);
#19115=ORIENTED_EDGE('',*,*,#14560,.T.);
#19116=ORIENTED_EDGE('',*,*,#14450,.F.);
#19117=ORIENTED_EDGE('',*,*,#14065,.F.);
#19118=ORIENTED_EDGE('',*,*,#13784,.F.);
#19119=ORIENTED_EDGE('',*,*,#14064,.T.);
#19120=ORIENTED_EDGE('',*,*,#14401,.F.);
#19121=ORIENTED_EDGE('',*,*,#14561,.F.);
#19122=ORIENTED_EDGE('',*,*,#13785,.F.);
#19123=ORIENTED_EDGE('',*,*,#14561,.T.);
#19124=ORIENTED_EDGE('',*,*,#14400,.F.);
#19125=ORIENTED_EDGE('',*,*,#14562,.F.);
#19126=ORIENTED_EDGE('',*,*,#13786,.F.);
#19127=ORIENTED_EDGE('',*,*,#14562,.T.);
#19128=ORIENTED_EDGE('',*,*,#14399,.F.);
#19129=ORIENTED_EDGE('',*,*,#14563,.F.);
#19130=ORIENTED_EDGE('',*,*,#13787,.F.);
#19131=ORIENTED_EDGE('',*,*,#14563,.T.);
#19132=ORIENTED_EDGE('',*,*,#14398,.F.);
#19133=ORIENTED_EDGE('',*,*,#14564,.F.);
#19134=ORIENTED_EDGE('',*,*,#13788,.F.);
#19135=ORIENTED_EDGE('',*,*,#14564,.T.);
#19136=ORIENTED_EDGE('',*,*,#14397,.F.);
#19137=ORIENTED_EDGE('',*,*,#14565,.F.);
#19138=ORIENTED_EDGE('',*,*,#13789,.F.);
#19139=ORIENTED_EDGE('',*,*,#14565,.T.);
#19140=ORIENTED_EDGE('',*,*,#14396,.F.);
#19141=ORIENTED_EDGE('',*,*,#14566,.F.);
#19142=ORIENTED_EDGE('',*,*,#13790,.F.);
#19143=ORIENTED_EDGE('',*,*,#14566,.T.);
#19144=ORIENTED_EDGE('',*,*,#14395,.F.);
#19145=ORIENTED_EDGE('',*,*,#14567,.F.);
#19146=ORIENTED_EDGE('',*,*,#13791,.F.);
#19147=ORIENTED_EDGE('',*,*,#14567,.T.);
#19148=ORIENTED_EDGE('',*,*,#14394,.F.);
#19149=ORIENTED_EDGE('',*,*,#14568,.F.);
#19150=ORIENTED_EDGE('',*,*,#13792,.F.);
#19151=ORIENTED_EDGE('',*,*,#14568,.T.);
#19152=ORIENTED_EDGE('',*,*,#14393,.F.);
#19153=ORIENTED_EDGE('',*,*,#14569,.F.);
#19154=ORIENTED_EDGE('',*,*,#13793,.F.);
#19155=ORIENTED_EDGE('',*,*,#14569,.T.);
#19156=ORIENTED_EDGE('',*,*,#14392,.F.);
#19157=ORIENTED_EDGE('',*,*,#14570,.F.);
#19158=ORIENTED_EDGE('',*,*,#13794,.F.);
#19159=ORIENTED_EDGE('',*,*,#14570,.T.);
#19160=ORIENTED_EDGE('',*,*,#14391,.F.);
#19161=ORIENTED_EDGE('',*,*,#14571,.F.);
#19162=ORIENTED_EDGE('',*,*,#13795,.F.);
#19163=ORIENTED_EDGE('',*,*,#14571,.T.);
#19164=ORIENTED_EDGE('',*,*,#14390,.F.);
#19165=ORIENTED_EDGE('',*,*,#14572,.F.);
#19166=ORIENTED_EDGE('',*,*,#13796,.F.);
#19167=ORIENTED_EDGE('',*,*,#14572,.T.);
#19168=ORIENTED_EDGE('',*,*,#14389,.F.);
#19169=ORIENTED_EDGE('',*,*,#14573,.F.);
#19170=ORIENTED_EDGE('',*,*,#13797,.F.);
#19171=ORIENTED_EDGE('',*,*,#14573,.T.);
#19172=ORIENTED_EDGE('',*,*,#14388,.F.);
#19173=ORIENTED_EDGE('',*,*,#14574,.F.);
#19174=ORIENTED_EDGE('',*,*,#14182,.F.);
#19175=ORIENTED_EDGE('',*,*,#13798,.F.);
#19176=ORIENTED_EDGE('',*,*,#14574,.T.);
#19177=ORIENTED_EDGE('',*,*,#14387,.F.);
#19178=ORIENTED_EDGE('',*,*,#14453,.F.);
#19179=ORIENTED_EDGE('',*,*,#14575,.F.);
#19180=ORIENTED_EDGE('',*,*,#14183,.F.);
#19181=ORIENTED_EDGE('',*,*,#14575,.T.);
#19182=ORIENTED_EDGE('',*,*,#14455,.F.);
#19183=ORIENTED_EDGE('',*,*,#14187,.F.);
#19184=ORIENTED_EDGE('',*,*,#13800,.F.);
#19185=ORIENTED_EDGE('',*,*,#14181,.F.);
#19186=ORIENTED_EDGE('',*,*,#14186,.T.);
#19187=ORIENTED_EDGE('',*,*,#14454,.F.);
#19188=ORIENTED_EDGE('',*,*,#14385,.F.);
#19189=ORIENTED_EDGE('',*,*,#14576,.F.);
#19190=ORIENTED_EDGE('',*,*,#13801,.F.);
#19191=ORIENTED_EDGE('',*,*,#14576,.T.);
#19192=ORIENTED_EDGE('',*,*,#14384,.F.);
#19193=ORIENTED_EDGE('',*,*,#14458,.F.);
#19194=ORIENTED_EDGE('',*,*,#14577,.F.);
#19195=ORIENTED_EDGE('',*,*,#14046,.F.);
#19196=ORIENTED_EDGE('',*,*,#14047,.F.);
#19197=ORIENTED_EDGE('',*,*,#14577,.T.);
#19198=ORIENTED_EDGE('',*,*,#14457,.F.);
#19199=ORIENTED_EDGE('',*,*,#14578,.F.);
#19200=ORIENTED_EDGE('',*,*,#14048,.F.);
#19201=ORIENTED_EDGE('',*,*,#14578,.T.);
#19202=ORIENTED_EDGE('',*,*,#14456,.F.);
#19203=ORIENTED_EDGE('',*,*,#14054,.F.);
#19204=ORIENTED_EDGE('',*,*,#13804,.F.);
#19205=ORIENTED_EDGE('',*,*,#14053,.T.);
#19206=ORIENTED_EDGE('',*,*,#14382,.F.);
#19207=ORIENTED_EDGE('',*,*,#14579,.F.);
#19208=ORIENTED_EDGE('',*,*,#13805,.F.);
#19209=ORIENTED_EDGE('',*,*,#14579,.T.);
#19210=ORIENTED_EDGE('',*,*,#14381,.F.);
#19211=ORIENTED_EDGE('',*,*,#14580,.F.);
#19212=ORIENTED_EDGE('',*,*,#13806,.F.);
#19213=ORIENTED_EDGE('',*,*,#14580,.T.);
#19214=ORIENTED_EDGE('',*,*,#14380,.F.);
#19215=ORIENTED_EDGE('',*,*,#14581,.F.);
#19216=ORIENTED_EDGE('',*,*,#13807,.F.);
#19217=ORIENTED_EDGE('',*,*,#14581,.T.);
#19218=ORIENTED_EDGE('',*,*,#14379,.F.);
#19219=ORIENTED_EDGE('',*,*,#14582,.F.);
#19220=ORIENTED_EDGE('',*,*,#13808,.F.);
#19221=ORIENTED_EDGE('',*,*,#14582,.T.);
#19222=ORIENTED_EDGE('',*,*,#14378,.F.);
#19223=ORIENTED_EDGE('',*,*,#14583,.F.);
#19224=ORIENTED_EDGE('',*,*,#13809,.F.);
#19225=ORIENTED_EDGE('',*,*,#14583,.T.);
#19226=ORIENTED_EDGE('',*,*,#14377,.F.);
#19227=ORIENTED_EDGE('',*,*,#14584,.F.);
#19228=ORIENTED_EDGE('',*,*,#13810,.F.);
#19229=ORIENTED_EDGE('',*,*,#14584,.T.);
#19230=ORIENTED_EDGE('',*,*,#14376,.F.);
#19231=ORIENTED_EDGE('',*,*,#14585,.F.);
#19232=ORIENTED_EDGE('',*,*,#13811,.F.);
#19233=ORIENTED_EDGE('',*,*,#14585,.T.);
#19234=ORIENTED_EDGE('',*,*,#14375,.F.);
#19235=ORIENTED_EDGE('',*,*,#14586,.F.);
#19236=ORIENTED_EDGE('',*,*,#13812,.F.);
#19237=ORIENTED_EDGE('',*,*,#14586,.T.);
#19238=ORIENTED_EDGE('',*,*,#14374,.F.);
#19239=ORIENTED_EDGE('',*,*,#14587,.F.);
#19240=ORIENTED_EDGE('',*,*,#13813,.F.);
#19241=ORIENTED_EDGE('',*,*,#14587,.T.);
#19242=ORIENTED_EDGE('',*,*,#14373,.F.);
#19243=ORIENTED_EDGE('',*,*,#14588,.F.);
#19244=ORIENTED_EDGE('',*,*,#13814,.F.);
#19245=ORIENTED_EDGE('',*,*,#14588,.T.);
#19246=ORIENTED_EDGE('',*,*,#14372,.F.);
#19247=ORIENTED_EDGE('',*,*,#14589,.F.);
#19248=ORIENTED_EDGE('',*,*,#13815,.F.);
#19249=ORIENTED_EDGE('',*,*,#14589,.T.);
#19250=ORIENTED_EDGE('',*,*,#14371,.F.);
#19251=ORIENTED_EDGE('',*,*,#14590,.F.);
#19252=ORIENTED_EDGE('',*,*,#13816,.F.);
#19253=ORIENTED_EDGE('',*,*,#14590,.T.);
#19254=ORIENTED_EDGE('',*,*,#14370,.F.);
#19255=ORIENTED_EDGE('',*,*,#14591,.F.);
#19256=ORIENTED_EDGE('',*,*,#13817,.F.);
#19257=ORIENTED_EDGE('',*,*,#14591,.T.);
#19258=ORIENTED_EDGE('',*,*,#14369,.F.);
#19259=ORIENTED_EDGE('',*,*,#14592,.F.);
#19260=ORIENTED_EDGE('',*,*,#14172,.F.);
#19261=ORIENTED_EDGE('',*,*,#13818,.F.);
#19262=ORIENTED_EDGE('',*,*,#14592,.T.);
#19263=ORIENTED_EDGE('',*,*,#14368,.F.);
#19264=ORIENTED_EDGE('',*,*,#14459,.F.);
#19265=ORIENTED_EDGE('',*,*,#14593,.F.);
#19266=ORIENTED_EDGE('',*,*,#14173,.F.);
#19267=ORIENTED_EDGE('',*,*,#14593,.T.);
#19268=ORIENTED_EDGE('',*,*,#14461,.F.);
#19269=ORIENTED_EDGE('',*,*,#14177,.F.);
#19270=ORIENTED_EDGE('',*,*,#13820,.F.);
#19271=ORIENTED_EDGE('',*,*,#14171,.F.);
#19272=ORIENTED_EDGE('',*,*,#14176,.T.);
#19273=ORIENTED_EDGE('',*,*,#14460,.F.);
#19274=ORIENTED_EDGE('',*,*,#14366,.F.);
#19275=ORIENTED_EDGE('',*,*,#14594,.F.);
#19276=ORIENTED_EDGE('',*,*,#13821,.F.);
#19277=ORIENTED_EDGE('',*,*,#14594,.T.);
#19278=ORIENTED_EDGE('',*,*,#14365,.F.);
#19279=ORIENTED_EDGE('',*,*,#14464,.F.);
#19280=ORIENTED_EDGE('',*,*,#14595,.F.);
#19281=ORIENTED_EDGE('',*,*,#14035,.F.);
#19282=ORIENTED_EDGE('',*,*,#14036,.F.);
#19283=ORIENTED_EDGE('',*,*,#14595,.T.);
#19284=ORIENTED_EDGE('',*,*,#14463,.F.);
#19285=ORIENTED_EDGE('',*,*,#14596,.F.);
#19286=ORIENTED_EDGE('',*,*,#14037,.F.);
#19287=ORIENTED_EDGE('',*,*,#14596,.T.);
#19288=ORIENTED_EDGE('',*,*,#14462,.F.);
#19289=ORIENTED_EDGE('',*,*,#14043,.F.);
#19290=ORIENTED_EDGE('',*,*,#13824,.F.);
#19291=ORIENTED_EDGE('',*,*,#14042,.T.);
#19292=ORIENTED_EDGE('',*,*,#14363,.F.);
#19293=ORIENTED_EDGE('',*,*,#14597,.F.);
#19294=ORIENTED_EDGE('',*,*,#13825,.F.);
#19295=ORIENTED_EDGE('',*,*,#14597,.T.);
#19296=ORIENTED_EDGE('',*,*,#14362,.F.);
#19297=ORIENTED_EDGE('',*,*,#14598,.F.);
#19298=ORIENTED_EDGE('',*,*,#13826,.F.);
#19299=ORIENTED_EDGE('',*,*,#14598,.T.);
#19300=ORIENTED_EDGE('',*,*,#14361,.F.);
#19301=ORIENTED_EDGE('',*,*,#14599,.F.);
#19302=ORIENTED_EDGE('',*,*,#13827,.F.);
#19303=ORIENTED_EDGE('',*,*,#14599,.T.);
#19304=ORIENTED_EDGE('',*,*,#14360,.F.);
#19305=ORIENTED_EDGE('',*,*,#14600,.F.);
#19306=ORIENTED_EDGE('',*,*,#13828,.F.);
#19307=ORIENTED_EDGE('',*,*,#14600,.T.);
#19308=ORIENTED_EDGE('',*,*,#14359,.F.);
#19309=ORIENTED_EDGE('',*,*,#14601,.F.);
#19310=ORIENTED_EDGE('',*,*,#13829,.F.);
#19311=ORIENTED_EDGE('',*,*,#14601,.T.);
#19312=ORIENTED_EDGE('',*,*,#14358,.F.);
#19313=ORIENTED_EDGE('',*,*,#14602,.F.);
#19314=ORIENTED_EDGE('',*,*,#13830,.F.);
#19315=ORIENTED_EDGE('',*,*,#14602,.T.);
#19316=ORIENTED_EDGE('',*,*,#14357,.F.);
#19317=ORIENTED_EDGE('',*,*,#14603,.F.);
#19318=ORIENTED_EDGE('',*,*,#13831,.F.);
#19319=ORIENTED_EDGE('',*,*,#14603,.T.);
#19320=ORIENTED_EDGE('',*,*,#14356,.F.);
#19321=ORIENTED_EDGE('',*,*,#14604,.F.);
#19322=ORIENTED_EDGE('',*,*,#13832,.F.);
#19323=ORIENTED_EDGE('',*,*,#14604,.T.);
#19324=ORIENTED_EDGE('',*,*,#14355,.F.);
#19325=ORIENTED_EDGE('',*,*,#14605,.F.);
#19326=ORIENTED_EDGE('',*,*,#13833,.F.);
#19327=ORIENTED_EDGE('',*,*,#14605,.T.);
#19328=ORIENTED_EDGE('',*,*,#14354,.F.);
#19329=ORIENTED_EDGE('',*,*,#14606,.F.);
#19330=ORIENTED_EDGE('',*,*,#13834,.F.);
#19331=ORIENTED_EDGE('',*,*,#14606,.T.);
#19332=ORIENTED_EDGE('',*,*,#14353,.F.);
#19333=ORIENTED_EDGE('',*,*,#14607,.F.);
#19334=ORIENTED_EDGE('',*,*,#13835,.F.);
#19335=ORIENTED_EDGE('',*,*,#14607,.T.);
#19336=ORIENTED_EDGE('',*,*,#14352,.F.);
#19337=ORIENTED_EDGE('',*,*,#14608,.F.);
#19338=ORIENTED_EDGE('',*,*,#13836,.F.);
#19339=ORIENTED_EDGE('',*,*,#14608,.T.);
#19340=ORIENTED_EDGE('',*,*,#14351,.F.);
#19341=ORIENTED_EDGE('',*,*,#14609,.F.);
#19342=ORIENTED_EDGE('',*,*,#13837,.F.);
#19343=ORIENTED_EDGE('',*,*,#14609,.T.);
#19344=ORIENTED_EDGE('',*,*,#14350,.F.);
#19345=ORIENTED_EDGE('',*,*,#14610,.F.);
#19346=ORIENTED_EDGE('',*,*,#14162,.F.);
#19347=ORIENTED_EDGE('',*,*,#13838,.F.);
#19348=ORIENTED_EDGE('',*,*,#14610,.T.);
#19349=ORIENTED_EDGE('',*,*,#14349,.F.);
#19350=ORIENTED_EDGE('',*,*,#14465,.F.);
#19351=ORIENTED_EDGE('',*,*,#14611,.F.);
#19352=ORIENTED_EDGE('',*,*,#14163,.F.);
#19353=ORIENTED_EDGE('',*,*,#14611,.T.);
#19354=ORIENTED_EDGE('',*,*,#14467,.F.);
#19355=ORIENTED_EDGE('',*,*,#14167,.F.);
#19356=ORIENTED_EDGE('',*,*,#13840,.F.);
#19357=ORIENTED_EDGE('',*,*,#14161,.F.);
#19358=ORIENTED_EDGE('',*,*,#14166,.T.);
#19359=ORIENTED_EDGE('',*,*,#14466,.F.);
#19360=ORIENTED_EDGE('',*,*,#14347,.F.);
#19361=ORIENTED_EDGE('',*,*,#14612,.F.);
#19362=ORIENTED_EDGE('',*,*,#13841,.F.);
#19363=ORIENTED_EDGE('',*,*,#14612,.T.);
#19364=ORIENTED_EDGE('',*,*,#14346,.F.);
#19365=ORIENTED_EDGE('',*,*,#14470,.F.);
#19366=ORIENTED_EDGE('',*,*,#14613,.F.);
#19367=ORIENTED_EDGE('',*,*,#14024,.F.);
#19368=ORIENTED_EDGE('',*,*,#14025,.F.);
#19369=ORIENTED_EDGE('',*,*,#14613,.T.);
#19370=ORIENTED_EDGE('',*,*,#14469,.F.);
#19371=ORIENTED_EDGE('',*,*,#14614,.F.);
#19372=ORIENTED_EDGE('',*,*,#14026,.F.);
#19373=ORIENTED_EDGE('',*,*,#14614,.T.);
#19374=ORIENTED_EDGE('',*,*,#14468,.F.);
#19375=ORIENTED_EDGE('',*,*,#14032,.F.);
#19376=ORIENTED_EDGE('',*,*,#13844,.F.);
#19377=ORIENTED_EDGE('',*,*,#14031,.T.);
#19378=ORIENTED_EDGE('',*,*,#14344,.F.);
#19379=ORIENTED_EDGE('',*,*,#14615,.F.);
#19380=ORIENTED_EDGE('',*,*,#13845,.F.);
#19381=ORIENTED_EDGE('',*,*,#14615,.T.);
#19382=ORIENTED_EDGE('',*,*,#14343,.F.);
#19383=ORIENTED_EDGE('',*,*,#14616,.F.);
#19384=ORIENTED_EDGE('',*,*,#13846,.F.);
#19385=ORIENTED_EDGE('',*,*,#14616,.T.);
#19386=ORIENTED_EDGE('',*,*,#14342,.F.);
#19387=ORIENTED_EDGE('',*,*,#14617,.F.);
#19388=ORIENTED_EDGE('',*,*,#13847,.F.);
#19389=ORIENTED_EDGE('',*,*,#14617,.T.);
#19390=ORIENTED_EDGE('',*,*,#14341,.F.);
#19391=ORIENTED_EDGE('',*,*,#14618,.F.);
#19392=ORIENTED_EDGE('',*,*,#13848,.F.);
#19393=ORIENTED_EDGE('',*,*,#14618,.T.);
#19394=ORIENTED_EDGE('',*,*,#14340,.F.);
#19395=ORIENTED_EDGE('',*,*,#14619,.F.);
#19396=ORIENTED_EDGE('',*,*,#13849,.F.);
#19397=ORIENTED_EDGE('',*,*,#14619,.T.);
#19398=ORIENTED_EDGE('',*,*,#14339,.F.);
#19399=ORIENTED_EDGE('',*,*,#14620,.F.);
#19400=ORIENTED_EDGE('',*,*,#13850,.F.);
#19401=ORIENTED_EDGE('',*,*,#14620,.T.);
#19402=ORIENTED_EDGE('',*,*,#14338,.F.);
#19403=ORIENTED_EDGE('',*,*,#14621,.F.);
#19404=ORIENTED_EDGE('',*,*,#13851,.F.);
#19405=ORIENTED_EDGE('',*,*,#14621,.T.);
#19406=ORIENTED_EDGE('',*,*,#14337,.F.);
#19407=ORIENTED_EDGE('',*,*,#14622,.F.);
#19408=ORIENTED_EDGE('',*,*,#13852,.F.);
#19409=ORIENTED_EDGE('',*,*,#14622,.T.);
#19410=ORIENTED_EDGE('',*,*,#14336,.F.);
#19411=ORIENTED_EDGE('',*,*,#14623,.F.);
#19412=ORIENTED_EDGE('',*,*,#13853,.F.);
#19413=ORIENTED_EDGE('',*,*,#14623,.T.);
#19414=ORIENTED_EDGE('',*,*,#14335,.F.);
#19415=ORIENTED_EDGE('',*,*,#14624,.F.);
#19416=ORIENTED_EDGE('',*,*,#13854,.F.);
#19417=ORIENTED_EDGE('',*,*,#14624,.T.);
#19418=ORIENTED_EDGE('',*,*,#14334,.F.);
#19419=ORIENTED_EDGE('',*,*,#14625,.F.);
#19420=ORIENTED_EDGE('',*,*,#13855,.F.);
#19421=ORIENTED_EDGE('',*,*,#14625,.T.);
#19422=ORIENTED_EDGE('',*,*,#14333,.F.);
#19423=ORIENTED_EDGE('',*,*,#14626,.F.);
#19424=ORIENTED_EDGE('',*,*,#13856,.F.);
#19425=ORIENTED_EDGE('',*,*,#14626,.T.);
#19426=ORIENTED_EDGE('',*,*,#14332,.F.);
#19427=ORIENTED_EDGE('',*,*,#14627,.F.);
#19428=ORIENTED_EDGE('',*,*,#13857,.F.);
#19429=ORIENTED_EDGE('',*,*,#14627,.T.);
#19430=ORIENTED_EDGE('',*,*,#14331,.F.);
#19431=ORIENTED_EDGE('',*,*,#14628,.F.);
#19432=ORIENTED_EDGE('',*,*,#14152,.F.);
#19433=ORIENTED_EDGE('',*,*,#13858,.F.);
#19434=ORIENTED_EDGE('',*,*,#14628,.T.);
#19435=ORIENTED_EDGE('',*,*,#14330,.F.);
#19436=ORIENTED_EDGE('',*,*,#14471,.F.);
#19437=ORIENTED_EDGE('',*,*,#14629,.F.);
#19438=ORIENTED_EDGE('',*,*,#14153,.F.);
#19439=ORIENTED_EDGE('',*,*,#14629,.T.);
#19440=ORIENTED_EDGE('',*,*,#14473,.F.);
#19441=ORIENTED_EDGE('',*,*,#14157,.F.);
#19442=ORIENTED_EDGE('',*,*,#13860,.F.);
#19443=ORIENTED_EDGE('',*,*,#14151,.F.);
#19444=ORIENTED_EDGE('',*,*,#14156,.T.);
#19445=ORIENTED_EDGE('',*,*,#14472,.F.);
#19446=ORIENTED_EDGE('',*,*,#14328,.F.);
#19447=ORIENTED_EDGE('',*,*,#14630,.F.);
#19448=ORIENTED_EDGE('',*,*,#13861,.F.);
#19449=ORIENTED_EDGE('',*,*,#14630,.T.);
#19450=ORIENTED_EDGE('',*,*,#14327,.F.);
#19451=ORIENTED_EDGE('',*,*,#14476,.F.);
#19452=ORIENTED_EDGE('',*,*,#14631,.F.);
#19453=ORIENTED_EDGE('',*,*,#14013,.F.);
#19454=ORIENTED_EDGE('',*,*,#14014,.F.);
#19455=ORIENTED_EDGE('',*,*,#14631,.T.);
#19456=ORIENTED_EDGE('',*,*,#14475,.F.);
#19457=ORIENTED_EDGE('',*,*,#14632,.F.);
#19458=ORIENTED_EDGE('',*,*,#14015,.F.);
#19459=ORIENTED_EDGE('',*,*,#14632,.T.);
#19460=ORIENTED_EDGE('',*,*,#14474,.F.);
#19461=ORIENTED_EDGE('',*,*,#14021,.F.);
#19462=ORIENTED_EDGE('',*,*,#13864,.F.);
#19463=ORIENTED_EDGE('',*,*,#14020,.T.);
#19464=ORIENTED_EDGE('',*,*,#14325,.F.);
#19465=ORIENTED_EDGE('',*,*,#14633,.F.);
#19466=ORIENTED_EDGE('',*,*,#13865,.F.);
#19467=ORIENTED_EDGE('',*,*,#14633,.T.);
#19468=ORIENTED_EDGE('',*,*,#14324,.F.);
#19469=ORIENTED_EDGE('',*,*,#14634,.F.);
#19470=ORIENTED_EDGE('',*,*,#13866,.F.);
#19471=ORIENTED_EDGE('',*,*,#14634,.T.);
#19472=ORIENTED_EDGE('',*,*,#14323,.F.);
#19473=ORIENTED_EDGE('',*,*,#14635,.F.);
#19474=ORIENTED_EDGE('',*,*,#13867,.F.);
#19475=ORIENTED_EDGE('',*,*,#14635,.T.);
#19476=ORIENTED_EDGE('',*,*,#14322,.F.);
#19477=ORIENTED_EDGE('',*,*,#14636,.F.);
#19478=ORIENTED_EDGE('',*,*,#13868,.F.);
#19479=ORIENTED_EDGE('',*,*,#14636,.T.);
#19480=ORIENTED_EDGE('',*,*,#14321,.F.);
#19481=ORIENTED_EDGE('',*,*,#14637,.F.);
#19482=ORIENTED_EDGE('',*,*,#13869,.F.);
#19483=ORIENTED_EDGE('',*,*,#14637,.T.);
#19484=ORIENTED_EDGE('',*,*,#14320,.F.);
#19485=ORIENTED_EDGE('',*,*,#14638,.F.);
#19486=ORIENTED_EDGE('',*,*,#13870,.F.);
#19487=ORIENTED_EDGE('',*,*,#14638,.T.);
#19488=ORIENTED_EDGE('',*,*,#14319,.F.);
#19489=ORIENTED_EDGE('',*,*,#14639,.F.);
#19490=ORIENTED_EDGE('',*,*,#13871,.F.);
#19491=ORIENTED_EDGE('',*,*,#14639,.T.);
#19492=ORIENTED_EDGE('',*,*,#14318,.F.);
#19493=ORIENTED_EDGE('',*,*,#14640,.F.);
#19494=ORIENTED_EDGE('',*,*,#13872,.F.);
#19495=ORIENTED_EDGE('',*,*,#14640,.T.);
#19496=ORIENTED_EDGE('',*,*,#14317,.F.);
#19497=ORIENTED_EDGE('',*,*,#14641,.F.);
#19498=ORIENTED_EDGE('',*,*,#13873,.F.);
#19499=ORIENTED_EDGE('',*,*,#14641,.T.);
#19500=ORIENTED_EDGE('',*,*,#14316,.F.);
#19501=ORIENTED_EDGE('',*,*,#14642,.F.);
#19502=ORIENTED_EDGE('',*,*,#13874,.F.);
#19503=ORIENTED_EDGE('',*,*,#14642,.T.);
#19504=ORIENTED_EDGE('',*,*,#14315,.F.);
#19505=ORIENTED_EDGE('',*,*,#14643,.F.);
#19506=ORIENTED_EDGE('',*,*,#13875,.F.);
#19507=ORIENTED_EDGE('',*,*,#14643,.T.);
#19508=ORIENTED_EDGE('',*,*,#14314,.F.);
#19509=ORIENTED_EDGE('',*,*,#14644,.F.);
#19510=ORIENTED_EDGE('',*,*,#13876,.F.);
#19511=ORIENTED_EDGE('',*,*,#14644,.T.);
#19512=ORIENTED_EDGE('',*,*,#14313,.F.);
#19513=ORIENTED_EDGE('',*,*,#14645,.F.);
#19514=ORIENTED_EDGE('',*,*,#13877,.F.);
#19515=ORIENTED_EDGE('',*,*,#14645,.T.);
#19516=ORIENTED_EDGE('',*,*,#14312,.F.);
#19517=ORIENTED_EDGE('',*,*,#14646,.F.);
#19518=ORIENTED_EDGE('',*,*,#14142,.F.);
#19519=ORIENTED_EDGE('',*,*,#13878,.F.);
#19520=ORIENTED_EDGE('',*,*,#14646,.T.);
#19521=ORIENTED_EDGE('',*,*,#14311,.F.);
#19522=ORIENTED_EDGE('',*,*,#14477,.F.);
#19523=ORIENTED_EDGE('',*,*,#14647,.F.);
#19524=ORIENTED_EDGE('',*,*,#14143,.F.);
#19525=ORIENTED_EDGE('',*,*,#14647,.T.);
#19526=ORIENTED_EDGE('',*,*,#14479,.F.);
#19527=ORIENTED_EDGE('',*,*,#14147,.F.);
#19528=ORIENTED_EDGE('',*,*,#13880,.F.);
#19529=ORIENTED_EDGE('',*,*,#14141,.F.);
#19530=ORIENTED_EDGE('',*,*,#14146,.T.);
#19531=ORIENTED_EDGE('',*,*,#14478,.F.);
#19532=ORIENTED_EDGE('',*,*,#14309,.F.);
#19533=ORIENTED_EDGE('',*,*,#14648,.F.);
#19534=ORIENTED_EDGE('',*,*,#13881,.F.);
#19535=ORIENTED_EDGE('',*,*,#14648,.T.);
#19536=ORIENTED_EDGE('',*,*,#14308,.F.);
#19537=ORIENTED_EDGE('',*,*,#14482,.F.);
#19538=ORIENTED_EDGE('',*,*,#14649,.F.);
#19539=ORIENTED_EDGE('',*,*,#14002,.F.);
#19540=ORIENTED_EDGE('',*,*,#14003,.F.);
#19541=ORIENTED_EDGE('',*,*,#14649,.T.);
#19542=ORIENTED_EDGE('',*,*,#14481,.F.);
#19543=ORIENTED_EDGE('',*,*,#14650,.F.);
#19544=ORIENTED_EDGE('',*,*,#14004,.F.);
#19545=ORIENTED_EDGE('',*,*,#14650,.T.);
#19546=ORIENTED_EDGE('',*,*,#14480,.F.);
#19547=ORIENTED_EDGE('',*,*,#14010,.F.);
#19548=ORIENTED_EDGE('',*,*,#13884,.F.);
#19549=ORIENTED_EDGE('',*,*,#14009,.T.);
#19550=ORIENTED_EDGE('',*,*,#14306,.F.);
#19551=ORIENTED_EDGE('',*,*,#14651,.F.);
#19552=ORIENTED_EDGE('',*,*,#13885,.F.);
#19553=ORIENTED_EDGE('',*,*,#14651,.T.);
#19554=ORIENTED_EDGE('',*,*,#14305,.F.);
#19555=ORIENTED_EDGE('',*,*,#14652,.F.);
#19556=ORIENTED_EDGE('',*,*,#13886,.F.);
#19557=ORIENTED_EDGE('',*,*,#14652,.T.);
#19558=ORIENTED_EDGE('',*,*,#14304,.F.);
#19559=ORIENTED_EDGE('',*,*,#14653,.F.);
#19560=ORIENTED_EDGE('',*,*,#13887,.F.);
#19561=ORIENTED_EDGE('',*,*,#14653,.T.);
#19562=ORIENTED_EDGE('',*,*,#14303,.F.);
#19563=ORIENTED_EDGE('',*,*,#14654,.F.);
#19564=ORIENTED_EDGE('',*,*,#13888,.F.);
#19565=ORIENTED_EDGE('',*,*,#14654,.T.);
#19566=ORIENTED_EDGE('',*,*,#14302,.F.);
#19567=ORIENTED_EDGE('',*,*,#14655,.F.);
#19568=ORIENTED_EDGE('',*,*,#13889,.F.);
#19569=ORIENTED_EDGE('',*,*,#14655,.T.);
#19570=ORIENTED_EDGE('',*,*,#14301,.F.);
#19571=ORIENTED_EDGE('',*,*,#14656,.F.);
#19572=ORIENTED_EDGE('',*,*,#13890,.F.);
#19573=ORIENTED_EDGE('',*,*,#14656,.T.);
#19574=ORIENTED_EDGE('',*,*,#14300,.F.);
#19575=ORIENTED_EDGE('',*,*,#14657,.F.);
#19576=ORIENTED_EDGE('',*,*,#13891,.F.);
#19577=ORIENTED_EDGE('',*,*,#14657,.T.);
#19578=ORIENTED_EDGE('',*,*,#14299,.F.);
#19579=ORIENTED_EDGE('',*,*,#14658,.F.);
#19580=ORIENTED_EDGE('',*,*,#13892,.F.);
#19581=ORIENTED_EDGE('',*,*,#14658,.T.);
#19582=ORIENTED_EDGE('',*,*,#14298,.F.);
#19583=ORIENTED_EDGE('',*,*,#14659,.F.);
#19584=ORIENTED_EDGE('',*,*,#13893,.F.);
#19585=ORIENTED_EDGE('',*,*,#14659,.T.);
#19586=ORIENTED_EDGE('',*,*,#14297,.F.);
#19587=ORIENTED_EDGE('',*,*,#14660,.F.);
#19588=ORIENTED_EDGE('',*,*,#13894,.F.);
#19589=ORIENTED_EDGE('',*,*,#14660,.T.);
#19590=ORIENTED_EDGE('',*,*,#14296,.F.);
#19591=ORIENTED_EDGE('',*,*,#14661,.F.);
#19592=ORIENTED_EDGE('',*,*,#13895,.F.);
#19593=ORIENTED_EDGE('',*,*,#14661,.T.);
#19594=ORIENTED_EDGE('',*,*,#14295,.F.);
#19595=ORIENTED_EDGE('',*,*,#14662,.F.);
#19596=ORIENTED_EDGE('',*,*,#13896,.F.);
#19597=ORIENTED_EDGE('',*,*,#14662,.T.);
#19598=ORIENTED_EDGE('',*,*,#14294,.F.);
#19599=ORIENTED_EDGE('',*,*,#14663,.F.);
#19600=ORIENTED_EDGE('',*,*,#13897,.F.);
#19601=ORIENTED_EDGE('',*,*,#14663,.T.);
#19602=ORIENTED_EDGE('',*,*,#14293,.F.);
#19603=ORIENTED_EDGE('',*,*,#14664,.F.);
#19604=ORIENTED_EDGE('',*,*,#14132,.F.);
#19605=ORIENTED_EDGE('',*,*,#13898,.F.);
#19606=ORIENTED_EDGE('',*,*,#14664,.T.);
#19607=ORIENTED_EDGE('',*,*,#14292,.F.);
#19608=ORIENTED_EDGE('',*,*,#14483,.F.);
#19609=ORIENTED_EDGE('',*,*,#14665,.F.);
#19610=ORIENTED_EDGE('',*,*,#14133,.F.);
#19611=ORIENTED_EDGE('',*,*,#14665,.T.);
#19612=ORIENTED_EDGE('',*,*,#14485,.F.);
#19613=ORIENTED_EDGE('',*,*,#14137,.F.);
#19614=ORIENTED_EDGE('',*,*,#13900,.F.);
#19615=ORIENTED_EDGE('',*,*,#14131,.F.);
#19616=ORIENTED_EDGE('',*,*,#14136,.T.);
#19617=ORIENTED_EDGE('',*,*,#14484,.F.);
#19618=ORIENTED_EDGE('',*,*,#14290,.F.);
#19619=ORIENTED_EDGE('',*,*,#14666,.F.);
#19620=ORIENTED_EDGE('',*,*,#13901,.F.);
#19621=ORIENTED_EDGE('',*,*,#14666,.T.);
#19622=ORIENTED_EDGE('',*,*,#14289,.F.);
#19623=ORIENTED_EDGE('',*,*,#14488,.F.);
#19624=ORIENTED_EDGE('',*,*,#14667,.F.);
#19625=ORIENTED_EDGE('',*,*,#13991,.F.);
#19626=ORIENTED_EDGE('',*,*,#13992,.F.);
#19627=ORIENTED_EDGE('',*,*,#14667,.T.);
#19628=ORIENTED_EDGE('',*,*,#14487,.F.);
#19629=ORIENTED_EDGE('',*,*,#14668,.F.);
#19630=ORIENTED_EDGE('',*,*,#13993,.F.);
#19631=ORIENTED_EDGE('',*,*,#14668,.T.);
#19632=ORIENTED_EDGE('',*,*,#14486,.F.);
#19633=ORIENTED_EDGE('',*,*,#13999,.F.);
#19634=ORIENTED_EDGE('',*,*,#13904,.F.);
#19635=ORIENTED_EDGE('',*,*,#13998,.T.);
#19636=ORIENTED_EDGE('',*,*,#14287,.F.);
#19637=ORIENTED_EDGE('',*,*,#14669,.F.);
#19638=ORIENTED_EDGE('',*,*,#13905,.F.);
#19639=ORIENTED_EDGE('',*,*,#14669,.T.);
#19640=ORIENTED_EDGE('',*,*,#14286,.F.);
#19641=ORIENTED_EDGE('',*,*,#14670,.F.);
#19642=ORIENTED_EDGE('',*,*,#13906,.F.);
#19643=ORIENTED_EDGE('',*,*,#14670,.T.);
#19644=ORIENTED_EDGE('',*,*,#14285,.F.);
#19645=ORIENTED_EDGE('',*,*,#14671,.F.);
#19646=ORIENTED_EDGE('',*,*,#13907,.F.);
#19647=ORIENTED_EDGE('',*,*,#14671,.T.);
#19648=ORIENTED_EDGE('',*,*,#14284,.F.);
#19649=ORIENTED_EDGE('',*,*,#14672,.F.);
#19650=ORIENTED_EDGE('',*,*,#13908,.F.);
#19651=ORIENTED_EDGE('',*,*,#14672,.T.);
#19652=ORIENTED_EDGE('',*,*,#14283,.F.);
#19653=ORIENTED_EDGE('',*,*,#14673,.F.);
#19654=ORIENTED_EDGE('',*,*,#13909,.F.);
#19655=ORIENTED_EDGE('',*,*,#14673,.T.);
#19656=ORIENTED_EDGE('',*,*,#14282,.F.);
#19657=ORIENTED_EDGE('',*,*,#14674,.F.);
#19658=ORIENTED_EDGE('',*,*,#13910,.F.);
#19659=ORIENTED_EDGE('',*,*,#14674,.T.);
#19660=ORIENTED_EDGE('',*,*,#14281,.F.);
#19661=ORIENTED_EDGE('',*,*,#14675,.F.);
#19662=ORIENTED_EDGE('',*,*,#13911,.F.);
#19663=ORIENTED_EDGE('',*,*,#14675,.T.);
#19664=ORIENTED_EDGE('',*,*,#14280,.F.);
#19665=ORIENTED_EDGE('',*,*,#14676,.F.);
#19666=ORIENTED_EDGE('',*,*,#13912,.F.);
#19667=ORIENTED_EDGE('',*,*,#14676,.T.);
#19668=ORIENTED_EDGE('',*,*,#14279,.F.);
#19669=ORIENTED_EDGE('',*,*,#14677,.F.);
#19670=ORIENTED_EDGE('',*,*,#13913,.F.);
#19671=ORIENTED_EDGE('',*,*,#14677,.T.);
#19672=ORIENTED_EDGE('',*,*,#14278,.F.);
#19673=ORIENTED_EDGE('',*,*,#14678,.F.);
#19674=ORIENTED_EDGE('',*,*,#13914,.F.);
#19675=ORIENTED_EDGE('',*,*,#14678,.T.);
#19676=ORIENTED_EDGE('',*,*,#14277,.F.);
#19677=ORIENTED_EDGE('',*,*,#14679,.F.);
#19678=ORIENTED_EDGE('',*,*,#13915,.F.);
#19679=ORIENTED_EDGE('',*,*,#14679,.T.);
#19680=ORIENTED_EDGE('',*,*,#14276,.F.);
#19681=ORIENTED_EDGE('',*,*,#14680,.F.);
#19682=ORIENTED_EDGE('',*,*,#13916,.F.);
#19683=ORIENTED_EDGE('',*,*,#14680,.T.);
#19684=ORIENTED_EDGE('',*,*,#14275,.F.);
#19685=ORIENTED_EDGE('',*,*,#14681,.F.);
#19686=ORIENTED_EDGE('',*,*,#13917,.F.);
#19687=ORIENTED_EDGE('',*,*,#14681,.T.);
#19688=ORIENTED_EDGE('',*,*,#14274,.F.);
#19689=ORIENTED_EDGE('',*,*,#14682,.F.);
#19690=ORIENTED_EDGE('',*,*,#14122,.F.);
#19691=ORIENTED_EDGE('',*,*,#13918,.F.);
#19692=ORIENTED_EDGE('',*,*,#14682,.T.);
#19693=ORIENTED_EDGE('',*,*,#14273,.F.);
#19694=ORIENTED_EDGE('',*,*,#14489,.F.);
#19695=ORIENTED_EDGE('',*,*,#14683,.F.);
#19696=ORIENTED_EDGE('',*,*,#14123,.F.);
#19697=ORIENTED_EDGE('',*,*,#14683,.T.);
#19698=ORIENTED_EDGE('',*,*,#14491,.F.);
#19699=ORIENTED_EDGE('',*,*,#14127,.F.);
#19700=ORIENTED_EDGE('',*,*,#13920,.F.);
#19701=ORIENTED_EDGE('',*,*,#14121,.F.);
#19702=ORIENTED_EDGE('',*,*,#14126,.T.);
#19703=ORIENTED_EDGE('',*,*,#14490,.F.);
#19704=ORIENTED_EDGE('',*,*,#14271,.F.);
#19705=ORIENTED_EDGE('',*,*,#14684,.F.);
#19706=ORIENTED_EDGE('',*,*,#13921,.F.);
#19707=ORIENTED_EDGE('',*,*,#14684,.T.);
#19708=ORIENTED_EDGE('',*,*,#14270,.F.);
#19709=ORIENTED_EDGE('',*,*,#14494,.F.);
#19710=ORIENTED_EDGE('',*,*,#14685,.F.);
#19711=ORIENTED_EDGE('',*,*,#13980,.F.);
#19712=ORIENTED_EDGE('',*,*,#13981,.F.);
#19713=ORIENTED_EDGE('',*,*,#14685,.T.);
#19714=ORIENTED_EDGE('',*,*,#14493,.F.);
#19715=ORIENTED_EDGE('',*,*,#14686,.F.);
#19716=ORIENTED_EDGE('',*,*,#13982,.F.);
#19717=ORIENTED_EDGE('',*,*,#14686,.T.);
#19718=ORIENTED_EDGE('',*,*,#14492,.F.);
#19719=ORIENTED_EDGE('',*,*,#13988,.F.);
#19720=ORIENTED_EDGE('',*,*,#13924,.F.);
#19721=ORIENTED_EDGE('',*,*,#13987,.T.);
#19722=ORIENTED_EDGE('',*,*,#14268,.F.);
#19723=ORIENTED_EDGE('',*,*,#14687,.F.);
#19724=ORIENTED_EDGE('',*,*,#13925,.F.);
#19725=ORIENTED_EDGE('',*,*,#14687,.T.);
#19726=ORIENTED_EDGE('',*,*,#14267,.F.);
#19727=ORIENTED_EDGE('',*,*,#14688,.F.);
#19728=ORIENTED_EDGE('',*,*,#13926,.F.);
#19729=ORIENTED_EDGE('',*,*,#14688,.T.);
#19730=ORIENTED_EDGE('',*,*,#14266,.F.);
#19731=ORIENTED_EDGE('',*,*,#14689,.F.);
#19732=ORIENTED_EDGE('',*,*,#13927,.F.);
#19733=ORIENTED_EDGE('',*,*,#14689,.T.);
#19734=ORIENTED_EDGE('',*,*,#14265,.F.);
#19735=ORIENTED_EDGE('',*,*,#14690,.F.);
#19736=ORIENTED_EDGE('',*,*,#13928,.F.);
#19737=ORIENTED_EDGE('',*,*,#14690,.T.);
#19738=ORIENTED_EDGE('',*,*,#14264,.F.);
#19739=ORIENTED_EDGE('',*,*,#14691,.F.);
#19740=ORIENTED_EDGE('',*,*,#13929,.F.);
#19741=ORIENTED_EDGE('',*,*,#14691,.T.);
#19742=ORIENTED_EDGE('',*,*,#14263,.F.);
#19743=ORIENTED_EDGE('',*,*,#14692,.F.);
#19744=ORIENTED_EDGE('',*,*,#13930,.F.);
#19745=ORIENTED_EDGE('',*,*,#14692,.T.);
#19746=ORIENTED_EDGE('',*,*,#14262,.F.);
#19747=ORIENTED_EDGE('',*,*,#14693,.F.);
#19748=ORIENTED_EDGE('',*,*,#13931,.F.);
#19749=ORIENTED_EDGE('',*,*,#14693,.T.);
#19750=ORIENTED_EDGE('',*,*,#14261,.F.);
#19751=ORIENTED_EDGE('',*,*,#14694,.F.);
#19752=ORIENTED_EDGE('',*,*,#13932,.F.);
#19753=ORIENTED_EDGE('',*,*,#14694,.T.);
#19754=ORIENTED_EDGE('',*,*,#14260,.F.);
#19755=ORIENTED_EDGE('',*,*,#14695,.F.);
#19756=ORIENTED_EDGE('',*,*,#13933,.F.);
#19757=ORIENTED_EDGE('',*,*,#14695,.T.);
#19758=ORIENTED_EDGE('',*,*,#14259,.F.);
#19759=ORIENTED_EDGE('',*,*,#14696,.F.);
#19760=ORIENTED_EDGE('',*,*,#13934,.F.);
#19761=ORIENTED_EDGE('',*,*,#14696,.T.);
#19762=ORIENTED_EDGE('',*,*,#14258,.F.);
#19763=ORIENTED_EDGE('',*,*,#14697,.F.);
#19764=ORIENTED_EDGE('',*,*,#13935,.F.);
#19765=ORIENTED_EDGE('',*,*,#14697,.T.);
#19766=ORIENTED_EDGE('',*,*,#14257,.F.);
#19767=ORIENTED_EDGE('',*,*,#14698,.F.);
#19768=ORIENTED_EDGE('',*,*,#13936,.F.);
#19769=ORIENTED_EDGE('',*,*,#14698,.T.);
#19770=ORIENTED_EDGE('',*,*,#14256,.F.);
#19771=ORIENTED_EDGE('',*,*,#14699,.F.);
#19772=ORIENTED_EDGE('',*,*,#13937,.F.);
#19773=ORIENTED_EDGE('',*,*,#14699,.T.);
#19774=ORIENTED_EDGE('',*,*,#14255,.F.);
#19775=ORIENTED_EDGE('',*,*,#14700,.F.);
#19776=ORIENTED_EDGE('',*,*,#14112,.F.);
#19777=ORIENTED_EDGE('',*,*,#13938,.F.);
#19778=ORIENTED_EDGE('',*,*,#14700,.T.);
#19779=ORIENTED_EDGE('',*,*,#14254,.F.);
#19780=ORIENTED_EDGE('',*,*,#14495,.F.);
#19781=ORIENTED_EDGE('',*,*,#14701,.F.);
#19782=ORIENTED_EDGE('',*,*,#14113,.F.);
#19783=ORIENTED_EDGE('',*,*,#14701,.T.);
#19784=ORIENTED_EDGE('',*,*,#14497,.F.);
#19785=ORIENTED_EDGE('',*,*,#14117,.F.);
#19786=ORIENTED_EDGE('',*,*,#13940,.F.);
#19787=ORIENTED_EDGE('',*,*,#14111,.F.);
#19788=ORIENTED_EDGE('',*,*,#14116,.T.);
#19789=ORIENTED_EDGE('',*,*,#14496,.F.);
#19790=ORIENTED_EDGE('',*,*,#14252,.F.);
#19791=ORIENTED_EDGE('',*,*,#14702,.F.);
#19792=ORIENTED_EDGE('',*,*,#13941,.F.);
#19793=ORIENTED_EDGE('',*,*,#14702,.T.);
#19794=ORIENTED_EDGE('',*,*,#14251,.F.);
#19795=ORIENTED_EDGE('',*,*,#14500,.F.);
#19796=ORIENTED_EDGE('',*,*,#14703,.F.);
#19797=ORIENTED_EDGE('',*,*,#13969,.F.);
#19798=ORIENTED_EDGE('',*,*,#13970,.F.);
#19799=ORIENTED_EDGE('',*,*,#14703,.T.);
#19800=ORIENTED_EDGE('',*,*,#14499,.F.);
#19801=ORIENTED_EDGE('',*,*,#14704,.F.);
#19802=ORIENTED_EDGE('',*,*,#13971,.F.);
#19803=ORIENTED_EDGE('',*,*,#14704,.T.);
#19804=ORIENTED_EDGE('',*,*,#14498,.F.);
#19805=ORIENTED_EDGE('',*,*,#13977,.F.);
#19806=ORIENTED_EDGE('',*,*,#13944,.F.);
#19807=ORIENTED_EDGE('',*,*,#13976,.T.);
#19808=ORIENTED_EDGE('',*,*,#14249,.F.);
#19809=ORIENTED_EDGE('',*,*,#14705,.F.);
#19810=ORIENTED_EDGE('',*,*,#13945,.F.);
#19811=ORIENTED_EDGE('',*,*,#14705,.T.);
#19812=ORIENTED_EDGE('',*,*,#14248,.F.);
#19813=ORIENTED_EDGE('',*,*,#14706,.F.);
#19814=ORIENTED_EDGE('',*,*,#13946,.F.);
#19815=ORIENTED_EDGE('',*,*,#14706,.T.);
#19816=ORIENTED_EDGE('',*,*,#14247,.F.);
#19817=ORIENTED_EDGE('',*,*,#14707,.F.);
#19818=ORIENTED_EDGE('',*,*,#13947,.F.);
#19819=ORIENTED_EDGE('',*,*,#14707,.T.);
#19820=ORIENTED_EDGE('',*,*,#14246,.F.);
#19821=ORIENTED_EDGE('',*,*,#14708,.F.);
#19822=ORIENTED_EDGE('',*,*,#13948,.F.);
#19823=ORIENTED_EDGE('',*,*,#14708,.T.);
#19824=ORIENTED_EDGE('',*,*,#14245,.F.);
#19825=ORIENTED_EDGE('',*,*,#14709,.F.);
#19826=ORIENTED_EDGE('',*,*,#13949,.F.);
#19827=ORIENTED_EDGE('',*,*,#14709,.T.);
#19828=ORIENTED_EDGE('',*,*,#14244,.F.);
#19829=ORIENTED_EDGE('',*,*,#14710,.F.);
#19830=ORIENTED_EDGE('',*,*,#13950,.F.);
#19831=ORIENTED_EDGE('',*,*,#14710,.T.);
#19832=ORIENTED_EDGE('',*,*,#14243,.F.);
#19833=ORIENTED_EDGE('',*,*,#14711,.F.);
#19834=ORIENTED_EDGE('',*,*,#13951,.F.);
#19835=ORIENTED_EDGE('',*,*,#14711,.T.);
#19836=ORIENTED_EDGE('',*,*,#14242,.F.);
#19837=ORIENTED_EDGE('',*,*,#14712,.F.);
#19838=ORIENTED_EDGE('',*,*,#13952,.F.);
#19839=ORIENTED_EDGE('',*,*,#14712,.T.);
#19840=ORIENTED_EDGE('',*,*,#14241,.F.);
#19841=ORIENTED_EDGE('',*,*,#14713,.F.);
#19842=ORIENTED_EDGE('',*,*,#13953,.F.);
#19843=ORIENTED_EDGE('',*,*,#14713,.T.);
#19844=ORIENTED_EDGE('',*,*,#14240,.F.);
#19845=ORIENTED_EDGE('',*,*,#14714,.F.);
#19846=ORIENTED_EDGE('',*,*,#13954,.F.);
#19847=ORIENTED_EDGE('',*,*,#14714,.T.);
#19848=ORIENTED_EDGE('',*,*,#14239,.F.);
#19849=ORIENTED_EDGE('',*,*,#14715,.F.);
#19850=ORIENTED_EDGE('',*,*,#13955,.F.);
#19851=ORIENTED_EDGE('',*,*,#14715,.T.);
#19852=ORIENTED_EDGE('',*,*,#14238,.F.);
#19853=ORIENTED_EDGE('',*,*,#14716,.F.);
#19854=ORIENTED_EDGE('',*,*,#13956,.F.);
#19855=ORIENTED_EDGE('',*,*,#14716,.T.);
#19856=ORIENTED_EDGE('',*,*,#14237,.F.);
#19857=ORIENTED_EDGE('',*,*,#14717,.F.);
#19858=ORIENTED_EDGE('',*,*,#13957,.F.);
#19859=ORIENTED_EDGE('',*,*,#14717,.T.);
#19860=ORIENTED_EDGE('',*,*,#14236,.F.);
#19861=ORIENTED_EDGE('',*,*,#14718,.F.);
#19862=ORIENTED_EDGE('',*,*,#14102,.F.);
#19863=ORIENTED_EDGE('',*,*,#13958,.F.);
#19864=ORIENTED_EDGE('',*,*,#14718,.T.);
#19865=ORIENTED_EDGE('',*,*,#14235,.F.);
#19866=ORIENTED_EDGE('',*,*,#14501,.F.);
#19867=ORIENTED_EDGE('',*,*,#14719,.F.);
#19868=ORIENTED_EDGE('',*,*,#14103,.F.);
#19869=ORIENTED_EDGE('',*,*,#14719,.T.);
#19870=ORIENTED_EDGE('',*,*,#14503,.F.);
#19871=ORIENTED_EDGE('',*,*,#14107,.F.);
#19872=ORIENTED_EDGE('',*,*,#13960,.F.);
#19873=ORIENTED_EDGE('',*,*,#14101,.F.);
#19874=ORIENTED_EDGE('',*,*,#14106,.T.);
#19875=ORIENTED_EDGE('',*,*,#14502,.F.);
#19876=ORIENTED_EDGE('',*,*,#14233,.F.);
#19877=ORIENTED_EDGE('',*,*,#14720,.F.);
#19878=ORIENTED_EDGE('',*,*,#13722,.F.);
#19879=ORIENTED_EDGE('',*,*,#14720,.T.);
#19880=ORIENTED_EDGE('',*,*,#14232,.F.);
#19881=ORIENTED_EDGE('',*,*,#14506,.F.);
#19882=ORIENTED_EDGE('',*,*,#14721,.F.);
#19883=ORIENTED_EDGE('',*,*,#13718,.F.);
#19884=ORIENTED_EDGE('',*,*,#13719,.F.);
#19885=ORIENTED_EDGE('',*,*,#14721,.T.);
#19886=ORIENTED_EDGE('',*,*,#14505,.F.);
#19887=ORIENTED_EDGE('',*,*,#14722,.F.);
#19888=ORIENTED_EDGE('',*,*,#13720,.F.);
#19889=ORIENTED_EDGE('',*,*,#14722,.T.);
#19890=ORIENTED_EDGE('',*,*,#14504,.F.);
#19891=ORIENTED_EDGE('',*,*,#13966,.F.);
#19892=ORIENTED_EDGE('',*,*,#13724,.F.);
#19893=ORIENTED_EDGE('',*,*,#13965,.T.);
#19894=ORIENTED_EDGE('',*,*,#14230,.F.);
#19895=ORIENTED_EDGE('',*,*,#14723,.F.);
#19896=ORIENTED_EDGE('',*,*,#13725,.F.);
#19897=ORIENTED_EDGE('',*,*,#14723,.T.);
#19898=ORIENTED_EDGE('',*,*,#14229,.F.);
#19899=ORIENTED_EDGE('',*,*,#14724,.F.);
#19900=ORIENTED_EDGE('',*,*,#13726,.F.);
#19901=ORIENTED_EDGE('',*,*,#14724,.T.);
#19902=ORIENTED_EDGE('',*,*,#14228,.F.);
#19903=ORIENTED_EDGE('',*,*,#14725,.F.);
#19904=ORIENTED_EDGE('',*,*,#13727,.F.);
#19905=ORIENTED_EDGE('',*,*,#14725,.T.);
#19906=ORIENTED_EDGE('',*,*,#14227,.F.);
#19907=ORIENTED_EDGE('',*,*,#14726,.F.);
#19908=ORIENTED_EDGE('',*,*,#13728,.F.);
#19909=ORIENTED_EDGE('',*,*,#14726,.T.);
#19910=ORIENTED_EDGE('',*,*,#14226,.F.);
#19911=ORIENTED_EDGE('',*,*,#14727,.F.);
#19912=ORIENTED_EDGE('',*,*,#13729,.F.);
#19913=ORIENTED_EDGE('',*,*,#14727,.T.);
#19914=ORIENTED_EDGE('',*,*,#14225,.F.);
#19915=ORIENTED_EDGE('',*,*,#14728,.F.);
#19916=ORIENTED_EDGE('',*,*,#13730,.F.);
#19917=ORIENTED_EDGE('',*,*,#14728,.T.);
#19918=ORIENTED_EDGE('',*,*,#14224,.F.);
#19919=ORIENTED_EDGE('',*,*,#14729,.F.);
#19920=ORIENTED_EDGE('',*,*,#13731,.F.);
#19921=ORIENTED_EDGE('',*,*,#14729,.T.);
#19922=ORIENTED_EDGE('',*,*,#14223,.F.);
#19923=ORIENTED_EDGE('',*,*,#14730,.F.);
#19924=ORIENTED_EDGE('',*,*,#13732,.F.);
#19925=ORIENTED_EDGE('',*,*,#14730,.T.);
#19926=ORIENTED_EDGE('',*,*,#14222,.F.);
#19927=ORIENTED_EDGE('',*,*,#14731,.F.);
#19928=ORIENTED_EDGE('',*,*,#13733,.F.);
#19929=ORIENTED_EDGE('',*,*,#14731,.T.);
#19930=ORIENTED_EDGE('',*,*,#14221,.F.);
#19931=ORIENTED_EDGE('',*,*,#14732,.F.);
#19932=ORIENTED_EDGE('',*,*,#13734,.F.);
#19933=ORIENTED_EDGE('',*,*,#14732,.T.);
#19934=ORIENTED_EDGE('',*,*,#14220,.F.);
#19935=ORIENTED_EDGE('',*,*,#14733,.F.);
#19936=ORIENTED_EDGE('',*,*,#13735,.F.);
#19937=ORIENTED_EDGE('',*,*,#14733,.T.);
#19938=ORIENTED_EDGE('',*,*,#14219,.F.);
#19939=ORIENTED_EDGE('',*,*,#14734,.F.);
#19940=ORIENTED_EDGE('',*,*,#13736,.F.);
#19941=ORIENTED_EDGE('',*,*,#14734,.T.);
#19942=ORIENTED_EDGE('',*,*,#14218,.F.);
#19943=ORIENTED_EDGE('',*,*,#14735,.F.);
#19944=ORIENTED_EDGE('',*,*,#13737,.F.);
#19945=ORIENTED_EDGE('',*,*,#14735,.T.);
#19946=ORIENTED_EDGE('',*,*,#14217,.F.);
#19947=ORIENTED_EDGE('',*,*,#14736,.F.);
#19948=ORIENTED_EDGE('',*,*,#14092,.F.);
#19949=ORIENTED_EDGE('',*,*,#13738,.F.);
#19950=ORIENTED_EDGE('',*,*,#14736,.T.);
#19951=ORIENTED_EDGE('',*,*,#14216,.F.);
#19952=ORIENTED_EDGE('',*,*,#14507,.F.);
#19953=ORIENTED_EDGE('',*,*,#14737,.F.);
#19954=ORIENTED_EDGE('',*,*,#14093,.F.);
#19955=ORIENTED_EDGE('',*,*,#14737,.T.);
#19956=ORIENTED_EDGE('',*,*,#14509,.F.);
#19957=ORIENTED_EDGE('',*,*,#14097,.F.);
#19958=ORIENTED_EDGE('',*,*,#13740,.F.);
#19959=ORIENTED_EDGE('',*,*,#14091,.F.);
#19960=ORIENTED_EDGE('',*,*,#14096,.T.);
#19961=ORIENTED_EDGE('',*,*,#14508,.F.);
#19962=ORIENTED_EDGE('',*,*,#14214,.F.);
#19963=ORIENTED_EDGE('',*,*,#14522,.F.);
#19964=ORIENTED_EDGE('',*,*,#13961,.T.);
#19965=ORIENTED_EDGE('',*,*,#14738,.T.);
#19966=ORIENTED_EDGE('',*,*,#14739,.T.);
#19967=ORIENTED_EDGE('',*,*,#14738,.F.);
#19968=ORIENTED_EDGE('',*,*,#14740,.F.);
#19969=ORIENTED_EDGE('',*,*,#14741,.F.);
#19970=ORIENTED_EDGE('',*,*,#14742,.T.);
#19971=ORIENTED_EDGE('',*,*,#14740,.T.);
#19972=ORIENTED_EDGE('',*,*,#14742,.F.);
#19973=ORIENTED_EDGE('',*,*,#14743,.F.);
#19974=ORIENTED_EDGE('',*,*,#14744,.T.);
#19975=ORIENTED_EDGE('',*,*,#14741,.T.);
#19976=ORIENTED_EDGE('',*,*,#14744,.F.);
#19977=ORIENTED_EDGE('',*,*,#14520,.T.);
#19978=ORIENTED_EDGE('',*,*,#14517,.T.);
#19979=ORIENTED_EDGE('',*,*,#14510,.T.);
#19980=ORIENTED_EDGE('',*,*,#14514,.T.);
#19981=ORIENTED_EDGE('',*,*,#14739,.F.);
#19982=ORIENTED_EDGE('',*,*,#14743,.T.);
#19983=ORIENTED_EDGE('',*,*,#14745,.F.);
#19984=ORIENTED_EDGE('',*,*,#14746,.T.);
#19985=ORIENTED_EDGE('',*,*,#14440,.T.);
#19986=ORIENTED_EDGE('',*,*,#14746,.F.);
#19987=ORIENTED_EDGE('',*,*,#14745,.T.);
#19988=ORIENTED_EDGE('',*,*,#14747,.T.);
#19989=ORIENTED_EDGE('',*,*,#14748,.T.);
#19990=ORIENTED_EDGE('',*,*,#14749,.T.);
#19991=ORIENTED_EDGE('',*,*,#14750,.T.);
#19992=ORIENTED_EDGE('',*,*,#14751,.T.);
#19993=ORIENTED_EDGE('',*,*,#14752,.T.);
#19994=ORIENTED_EDGE('',*,*,#14753,.T.);
#19995=ORIENTED_EDGE('',*,*,#14748,.F.);
#19996=ORIENTED_EDGE('',*,*,#14754,.T.);
#19997=ORIENTED_EDGE('',*,*,#14755,.T.);
#19998=ORIENTED_EDGE('',*,*,#14756,.T.);
#19999=ORIENTED_EDGE('',*,*,#14757,.T.);
#20000=ORIENTED_EDGE('',*,*,#14758,.T.);
#20001=ORIENTED_EDGE('',*,*,#14759,.T.);
#20002=ORIENTED_EDGE('',*,*,#14760,.T.);
#20003=ORIENTED_EDGE('',*,*,#14761,.T.);
#20004=ORIENTED_EDGE('',*,*,#14762,.T.);
#20005=ORIENTED_EDGE('',*,*,#14763,.T.);
#20006=ORIENTED_EDGE('',*,*,#14764,.T.);
#20007=ORIENTED_EDGE('',*,*,#14765,.T.);
#20008=ORIENTED_EDGE('',*,*,#14766,.T.);
#20009=ORIENTED_EDGE('',*,*,#14767,.T.);
#20010=ORIENTED_EDGE('',*,*,#14768,.T.);
#20011=ORIENTED_EDGE('',*,*,#14769,.T.);
#20012=ORIENTED_EDGE('',*,*,#14770,.F.);
#20013=ORIENTED_EDGE('',*,*,#14771,.T.);
#20014=ORIENTED_EDGE('',*,*,#14772,.T.);
#20015=ORIENTED_EDGE('',*,*,#14773,.F.);
#20016=ORIENTED_EDGE('',*,*,#14774,.T.);
#20017=ORIENTED_EDGE('',*,*,#14775,.T.);
#20018=ORIENTED_EDGE('',*,*,#14776,.T.);
#20019=ORIENTED_EDGE('',*,*,#14777,.T.);
#20020=ORIENTED_EDGE('',*,*,#14778,.T.);
#20021=ORIENTED_EDGE('',*,*,#14779,.T.);
#20022=ORIENTED_EDGE('',*,*,#14780,.T.);
#20023=ORIENTED_EDGE('',*,*,#14781,.T.);
#20024=ORIENTED_EDGE('',*,*,#14782,.T.);
#20025=ORIENTED_EDGE('',*,*,#14783,.T.);
#20026=ORIENTED_EDGE('',*,*,#14784,.T.);
#20027=ORIENTED_EDGE('',*,*,#14785,.T.);
#20028=ORIENTED_EDGE('',*,*,#14786,.T.);
#20029=ORIENTED_EDGE('',*,*,#14787,.T.);
#20030=ORIENTED_EDGE('',*,*,#14788,.T.);
#20031=ORIENTED_EDGE('',*,*,#14789,.T.);
#20032=ORIENTED_EDGE('',*,*,#14790,.F.);
#20033=ORIENTED_EDGE('',*,*,#14791,.T.);
#20034=ORIENTED_EDGE('',*,*,#14792,.T.);
#20035=ORIENTED_EDGE('',*,*,#14793,.F.);
#20036=ORIENTED_EDGE('',*,*,#14794,.T.);
#20037=ORIENTED_EDGE('',*,*,#14795,.T.);
#20038=ORIENTED_EDGE('',*,*,#14796,.T.);
#20039=ORIENTED_EDGE('',*,*,#14797,.T.);
#20040=ORIENTED_EDGE('',*,*,#14798,.T.);
#20041=ORIENTED_EDGE('',*,*,#14799,.T.);
#20042=ORIENTED_EDGE('',*,*,#14800,.T.);
#20043=ORIENTED_EDGE('',*,*,#14801,.T.);
#20044=ORIENTED_EDGE('',*,*,#14802,.T.);
#20045=ORIENTED_EDGE('',*,*,#14803,.T.);
#20046=ORIENTED_EDGE('',*,*,#14804,.T.);
#20047=ORIENTED_EDGE('',*,*,#14805,.T.);
#20048=ORIENTED_EDGE('',*,*,#14806,.T.);
#20049=ORIENTED_EDGE('',*,*,#14807,.T.);
#20050=ORIENTED_EDGE('',*,*,#14808,.T.);
#20051=ORIENTED_EDGE('',*,*,#14809,.T.);
#20052=ORIENTED_EDGE('',*,*,#14810,.F.);
#20053=ORIENTED_EDGE('',*,*,#14811,.T.);
#20054=ORIENTED_EDGE('',*,*,#14812,.T.);
#20055=ORIENTED_EDGE('',*,*,#14813,.F.);
#20056=ORIENTED_EDGE('',*,*,#14814,.T.);
#20057=ORIENTED_EDGE('',*,*,#14815,.T.);
#20058=ORIENTED_EDGE('',*,*,#14816,.T.);
#20059=ORIENTED_EDGE('',*,*,#14817,.T.);
#20060=ORIENTED_EDGE('',*,*,#14818,.T.);
#20061=ORIENTED_EDGE('',*,*,#14819,.T.);
#20062=ORIENTED_EDGE('',*,*,#14820,.T.);
#20063=ORIENTED_EDGE('',*,*,#14821,.T.);
#20064=ORIENTED_EDGE('',*,*,#14822,.T.);
#20065=ORIENTED_EDGE('',*,*,#14823,.T.);
#20066=ORIENTED_EDGE('',*,*,#14824,.T.);
#20067=ORIENTED_EDGE('',*,*,#14825,.T.);
#20068=ORIENTED_EDGE('',*,*,#14826,.T.);
#20069=ORIENTED_EDGE('',*,*,#14827,.T.);
#20070=ORIENTED_EDGE('',*,*,#14828,.T.);
#20071=ORIENTED_EDGE('',*,*,#14829,.T.);
#20072=ORIENTED_EDGE('',*,*,#14830,.F.);
#20073=ORIENTED_EDGE('',*,*,#14831,.T.);
#20074=ORIENTED_EDGE('',*,*,#14832,.T.);
#20075=ORIENTED_EDGE('',*,*,#14833,.F.);
#20076=ORIENTED_EDGE('',*,*,#14834,.T.);
#20077=ORIENTED_EDGE('',*,*,#14835,.T.);
#20078=ORIENTED_EDGE('',*,*,#14836,.T.);
#20079=ORIENTED_EDGE('',*,*,#14837,.T.);
#20080=ORIENTED_EDGE('',*,*,#14838,.T.);
#20081=ORIENTED_EDGE('',*,*,#14839,.T.);
#20082=ORIENTED_EDGE('',*,*,#14840,.T.);
#20083=ORIENTED_EDGE('',*,*,#14841,.T.);
#20084=ORIENTED_EDGE('',*,*,#14842,.T.);
#20085=ORIENTED_EDGE('',*,*,#14843,.T.);
#20086=ORIENTED_EDGE('',*,*,#14844,.T.);
#20087=ORIENTED_EDGE('',*,*,#14845,.T.);
#20088=ORIENTED_EDGE('',*,*,#14846,.T.);
#20089=ORIENTED_EDGE('',*,*,#14847,.T.);
#20090=ORIENTED_EDGE('',*,*,#14848,.T.);
#20091=ORIENTED_EDGE('',*,*,#14849,.T.);
#20092=ORIENTED_EDGE('',*,*,#14850,.F.);
#20093=ORIENTED_EDGE('',*,*,#14851,.T.);
#20094=ORIENTED_EDGE('',*,*,#14852,.T.);
#20095=ORIENTED_EDGE('',*,*,#14853,.F.);
#20096=ORIENTED_EDGE('',*,*,#14854,.T.);
#20097=ORIENTED_EDGE('',*,*,#14855,.T.);
#20098=ORIENTED_EDGE('',*,*,#14856,.T.);
#20099=ORIENTED_EDGE('',*,*,#14857,.T.);
#20100=ORIENTED_EDGE('',*,*,#14858,.T.);
#20101=ORIENTED_EDGE('',*,*,#14859,.T.);
#20102=ORIENTED_EDGE('',*,*,#14860,.T.);
#20103=ORIENTED_EDGE('',*,*,#14861,.T.);
#20104=ORIENTED_EDGE('',*,*,#14862,.T.);
#20105=ORIENTED_EDGE('',*,*,#14863,.T.);
#20106=ORIENTED_EDGE('',*,*,#14864,.T.);
#20107=ORIENTED_EDGE('',*,*,#14865,.T.);
#20108=ORIENTED_EDGE('',*,*,#14866,.T.);
#20109=ORIENTED_EDGE('',*,*,#14867,.T.);
#20110=ORIENTED_EDGE('',*,*,#14868,.T.);
#20111=ORIENTED_EDGE('',*,*,#14869,.T.);
#20112=ORIENTED_EDGE('',*,*,#14870,.F.);
#20113=ORIENTED_EDGE('',*,*,#14871,.T.);
#20114=ORIENTED_EDGE('',*,*,#14872,.T.);
#20115=ORIENTED_EDGE('',*,*,#14873,.F.);
#20116=ORIENTED_EDGE('',*,*,#14874,.T.);
#20117=ORIENTED_EDGE('',*,*,#14875,.T.);
#20118=ORIENTED_EDGE('',*,*,#14876,.T.);
#20119=ORIENTED_EDGE('',*,*,#14877,.T.);
#20120=ORIENTED_EDGE('',*,*,#14878,.T.);
#20121=ORIENTED_EDGE('',*,*,#14879,.T.);
#20122=ORIENTED_EDGE('',*,*,#14880,.T.);
#20123=ORIENTED_EDGE('',*,*,#14881,.T.);
#20124=ORIENTED_EDGE('',*,*,#14882,.T.);
#20125=ORIENTED_EDGE('',*,*,#14883,.T.);
#20126=ORIENTED_EDGE('',*,*,#14884,.T.);
#20127=ORIENTED_EDGE('',*,*,#14885,.T.);
#20128=ORIENTED_EDGE('',*,*,#14886,.T.);
#20129=ORIENTED_EDGE('',*,*,#14887,.T.);
#20130=ORIENTED_EDGE('',*,*,#14888,.T.);
#20131=ORIENTED_EDGE('',*,*,#14889,.T.);
#20132=ORIENTED_EDGE('',*,*,#14890,.F.);
#20133=ORIENTED_EDGE('',*,*,#14891,.T.);
#20134=ORIENTED_EDGE('',*,*,#14892,.T.);
#20135=ORIENTED_EDGE('',*,*,#14893,.F.);
#20136=ORIENTED_EDGE('',*,*,#14894,.T.);
#20137=ORIENTED_EDGE('',*,*,#14895,.T.);
#20138=ORIENTED_EDGE('',*,*,#14896,.T.);
#20139=ORIENTED_EDGE('',*,*,#14897,.T.);
#20140=ORIENTED_EDGE('',*,*,#14898,.T.);
#20141=ORIENTED_EDGE('',*,*,#14899,.T.);
#20142=ORIENTED_EDGE('',*,*,#14900,.T.);
#20143=ORIENTED_EDGE('',*,*,#14901,.T.);
#20144=ORIENTED_EDGE('',*,*,#14902,.T.);
#20145=ORIENTED_EDGE('',*,*,#14903,.T.);
#20146=ORIENTED_EDGE('',*,*,#14904,.T.);
#20147=ORIENTED_EDGE('',*,*,#14905,.T.);
#20148=ORIENTED_EDGE('',*,*,#14906,.T.);
#20149=ORIENTED_EDGE('',*,*,#14907,.T.);
#20150=ORIENTED_EDGE('',*,*,#14908,.T.);
#20151=ORIENTED_EDGE('',*,*,#14909,.T.);
#20152=ORIENTED_EDGE('',*,*,#14910,.F.);
#20153=ORIENTED_EDGE('',*,*,#14911,.T.);
#20154=ORIENTED_EDGE('',*,*,#14912,.T.);
#20155=ORIENTED_EDGE('',*,*,#14913,.F.);
#20156=ORIENTED_EDGE('',*,*,#14914,.T.);
#20157=ORIENTED_EDGE('',*,*,#14915,.T.);
#20158=ORIENTED_EDGE('',*,*,#14916,.T.);
#20159=ORIENTED_EDGE('',*,*,#14917,.T.);
#20160=ORIENTED_EDGE('',*,*,#14918,.T.);
#20161=ORIENTED_EDGE('',*,*,#14919,.T.);
#20162=ORIENTED_EDGE('',*,*,#14920,.T.);
#20163=ORIENTED_EDGE('',*,*,#14921,.T.);
#20164=ORIENTED_EDGE('',*,*,#14922,.T.);
#20165=ORIENTED_EDGE('',*,*,#14923,.T.);
#20166=ORIENTED_EDGE('',*,*,#14924,.T.);
#20167=ORIENTED_EDGE('',*,*,#14925,.T.);
#20168=ORIENTED_EDGE('',*,*,#14926,.T.);
#20169=ORIENTED_EDGE('',*,*,#14927,.T.);
#20170=ORIENTED_EDGE('',*,*,#14928,.T.);
#20171=ORIENTED_EDGE('',*,*,#14929,.T.);
#20172=ORIENTED_EDGE('',*,*,#14930,.F.);
#20173=ORIENTED_EDGE('',*,*,#14931,.T.);
#20174=ORIENTED_EDGE('',*,*,#14932,.T.);
#20175=ORIENTED_EDGE('',*,*,#14933,.F.);
#20176=ORIENTED_EDGE('',*,*,#14934,.T.);
#20177=ORIENTED_EDGE('',*,*,#14935,.T.);
#20178=ORIENTED_EDGE('',*,*,#14936,.T.);
#20179=ORIENTED_EDGE('',*,*,#14937,.T.);
#20180=ORIENTED_EDGE('',*,*,#14938,.T.);
#20181=ORIENTED_EDGE('',*,*,#14939,.T.);
#20182=ORIENTED_EDGE('',*,*,#14940,.T.);
#20183=ORIENTED_EDGE('',*,*,#14941,.T.);
#20184=ORIENTED_EDGE('',*,*,#14942,.T.);
#20185=ORIENTED_EDGE('',*,*,#14943,.T.);
#20186=ORIENTED_EDGE('',*,*,#14944,.T.);
#20187=ORIENTED_EDGE('',*,*,#14945,.T.);
#20188=ORIENTED_EDGE('',*,*,#14946,.T.);
#20189=ORIENTED_EDGE('',*,*,#14947,.T.);
#20190=ORIENTED_EDGE('',*,*,#14948,.T.);
#20191=ORIENTED_EDGE('',*,*,#14949,.T.);
#20192=ORIENTED_EDGE('',*,*,#14950,.F.);
#20193=ORIENTED_EDGE('',*,*,#14951,.T.);
#20194=ORIENTED_EDGE('',*,*,#14952,.T.);
#20195=ORIENTED_EDGE('',*,*,#14953,.F.);
#20196=ORIENTED_EDGE('',*,*,#14954,.T.);
#20197=ORIENTED_EDGE('',*,*,#14955,.T.);
#20198=ORIENTED_EDGE('',*,*,#14956,.T.);
#20199=ORIENTED_EDGE('',*,*,#14957,.T.);
#20200=ORIENTED_EDGE('',*,*,#14958,.T.);
#20201=ORIENTED_EDGE('',*,*,#14959,.T.);
#20202=ORIENTED_EDGE('',*,*,#14960,.T.);
#20203=ORIENTED_EDGE('',*,*,#14961,.T.);
#20204=ORIENTED_EDGE('',*,*,#14962,.T.);
#20205=ORIENTED_EDGE('',*,*,#14963,.T.);
#20206=ORIENTED_EDGE('',*,*,#14964,.T.);
#20207=ORIENTED_EDGE('',*,*,#14965,.T.);
#20208=ORIENTED_EDGE('',*,*,#14966,.T.);
#20209=ORIENTED_EDGE('',*,*,#14967,.T.);
#20210=ORIENTED_EDGE('',*,*,#14968,.T.);
#20211=ORIENTED_EDGE('',*,*,#14969,.T.);
#20212=ORIENTED_EDGE('',*,*,#14970,.F.);
#20213=ORIENTED_EDGE('',*,*,#14971,.T.);
#20214=ORIENTED_EDGE('',*,*,#14972,.T.);
#20215=ORIENTED_EDGE('',*,*,#14973,.F.);
#20216=ORIENTED_EDGE('',*,*,#14974,.T.);
#20217=ORIENTED_EDGE('',*,*,#14975,.T.);
#20218=ORIENTED_EDGE('',*,*,#14976,.T.);
#20219=ORIENTED_EDGE('',*,*,#14977,.T.);
#20220=ORIENTED_EDGE('',*,*,#14978,.T.);
#20221=ORIENTED_EDGE('',*,*,#14979,.T.);
#20222=ORIENTED_EDGE('',*,*,#14980,.T.);
#20223=ORIENTED_EDGE('',*,*,#14981,.T.);
#20224=ORIENTED_EDGE('',*,*,#14982,.T.);
#20225=ORIENTED_EDGE('',*,*,#14983,.T.);
#20226=ORIENTED_EDGE('',*,*,#14984,.T.);
#20227=ORIENTED_EDGE('',*,*,#14985,.T.);
#20228=ORIENTED_EDGE('',*,*,#14986,.T.);
#20229=ORIENTED_EDGE('',*,*,#14987,.T.);
#20230=ORIENTED_EDGE('',*,*,#14988,.T.);
#20231=ORIENTED_EDGE('',*,*,#14989,.T.);
#20232=ORIENTED_EDGE('',*,*,#14990,.F.);
#20233=ORIENTED_EDGE('',*,*,#14991,.T.);
#20234=ORIENTED_EDGE('',*,*,#14992,.F.);
#20235=ORIENTED_EDGE('',*,*,#14747,.F.);
#20236=ORIENTED_EDGE('',*,*,#14993,.T.);
#20237=ORIENTED_EDGE('',*,*,#14994,.F.);
#20238=ORIENTED_EDGE('',*,*,#14995,.F.);
#20239=ORIENTED_EDGE('',*,*,#14996,.F.);
#20240=ORIENTED_EDGE('',*,*,#14754,.F.);
#20241=ORIENTED_EDGE('',*,*,#14752,.F.);
#20242=ORIENTED_EDGE('',*,*,#14997,.T.);
#20243=ORIENTED_EDGE('',*,*,#14998,.F.);
#20244=ORIENTED_EDGE('',*,*,#14993,.F.);
#20245=ORIENTED_EDGE('',*,*,#14999,.T.);
#20246=ORIENTED_EDGE('',*,*,#14973,.T.);
#20247=ORIENTED_EDGE('',*,*,#15000,.T.);
#20248=ORIENTED_EDGE('',*,*,#15001,.T.);
#20249=ORIENTED_EDGE('',*,*,#15002,.T.);
#20250=ORIENTED_EDGE('',*,*,#15003,.T.);
#20251=ORIENTED_EDGE('',*,*,#14999,.F.);
#20252=ORIENTED_EDGE('',*,*,#15004,.T.);
#20253=ORIENTED_EDGE('',*,*,#15005,.F.);
#20254=ORIENTED_EDGE('',*,*,#15006,.F.);
#20255=ORIENTED_EDGE('',*,*,#15007,.F.);
#20256=ORIENTED_EDGE('',*,*,#14974,.F.);
#20257=ORIENTED_EDGE('',*,*,#15003,.F.);
#20258=ORIENTED_EDGE('',*,*,#15008,.T.);
#20259=ORIENTED_EDGE('',*,*,#15009,.F.);
#20260=ORIENTED_EDGE('',*,*,#15004,.F.);
#20261=ORIENTED_EDGE('',*,*,#15010,.T.);
#20262=ORIENTED_EDGE('',*,*,#14953,.T.);
#20263=ORIENTED_EDGE('',*,*,#15011,.T.);
#20264=ORIENTED_EDGE('',*,*,#15012,.T.);
#20265=ORIENTED_EDGE('',*,*,#15013,.T.);
#20266=ORIENTED_EDGE('',*,*,#15014,.T.);
#20267=ORIENTED_EDGE('',*,*,#15010,.F.);
#20268=ORIENTED_EDGE('',*,*,#15015,.T.);
#20269=ORIENTED_EDGE('',*,*,#15016,.F.);
#20270=ORIENTED_EDGE('',*,*,#15017,.F.);
#20271=ORIENTED_EDGE('',*,*,#15018,.F.);
#20272=ORIENTED_EDGE('',*,*,#14954,.F.);
#20273=ORIENTED_EDGE('',*,*,#15014,.F.);
#20274=ORIENTED_EDGE('',*,*,#15019,.T.);
#20275=ORIENTED_EDGE('',*,*,#15020,.F.);
#20276=ORIENTED_EDGE('',*,*,#15015,.F.);
#20277=ORIENTED_EDGE('',*,*,#15021,.T.);
#20278=ORIENTED_EDGE('',*,*,#14933,.T.);
#20279=ORIENTED_EDGE('',*,*,#15022,.T.);
#20280=ORIENTED_EDGE('',*,*,#15023,.T.);
#20281=ORIENTED_EDGE('',*,*,#15024,.T.);
#20282=ORIENTED_EDGE('',*,*,#15025,.T.);
#20283=ORIENTED_EDGE('',*,*,#15021,.F.);
#20284=ORIENTED_EDGE('',*,*,#15026,.T.);
#20285=ORIENTED_EDGE('',*,*,#15027,.F.);
#20286=ORIENTED_EDGE('',*,*,#15028,.F.);
#20287=ORIENTED_EDGE('',*,*,#15029,.F.);
#20288=ORIENTED_EDGE('',*,*,#14934,.F.);
#20289=ORIENTED_EDGE('',*,*,#15025,.F.);
#20290=ORIENTED_EDGE('',*,*,#15030,.T.);
#20291=ORIENTED_EDGE('',*,*,#15031,.F.);
#20292=ORIENTED_EDGE('',*,*,#15026,.F.);
#20293=ORIENTED_EDGE('',*,*,#15032,.T.);
#20294=ORIENTED_EDGE('',*,*,#14913,.T.);
#20295=ORIENTED_EDGE('',*,*,#15033,.T.);
#20296=ORIENTED_EDGE('',*,*,#15034,.T.);
#20297=ORIENTED_EDGE('',*,*,#15035,.T.);
#20298=ORIENTED_EDGE('',*,*,#15036,.T.);
#20299=ORIENTED_EDGE('',*,*,#15032,.F.);
#20300=ORIENTED_EDGE('',*,*,#15037,.T.);
#20301=ORIENTED_EDGE('',*,*,#15038,.F.);
#20302=ORIENTED_EDGE('',*,*,#15039,.F.);
#20303=ORIENTED_EDGE('',*,*,#15040,.F.);
#20304=ORIENTED_EDGE('',*,*,#14914,.F.);
#20305=ORIENTED_EDGE('',*,*,#15036,.F.);
#20306=ORIENTED_EDGE('',*,*,#15041,.T.);
#20307=ORIENTED_EDGE('',*,*,#15042,.F.);
#20308=ORIENTED_EDGE('',*,*,#15037,.F.);
#20309=ORIENTED_EDGE('',*,*,#15043,.T.);
#20310=ORIENTED_EDGE('',*,*,#14893,.T.);
#20311=ORIENTED_EDGE('',*,*,#15044,.T.);
#20312=ORIENTED_EDGE('',*,*,#15045,.T.);
#20313=ORIENTED_EDGE('',*,*,#15046,.T.);
#20314=ORIENTED_EDGE('',*,*,#15047,.T.);
#20315=ORIENTED_EDGE('',*,*,#15043,.F.);
#20316=ORIENTED_EDGE('',*,*,#15048,.T.);
#20317=ORIENTED_EDGE('',*,*,#15049,.F.);
#20318=ORIENTED_EDGE('',*,*,#15050,.F.);
#20319=ORIENTED_EDGE('',*,*,#15051,.F.);
#20320=ORIENTED_EDGE('',*,*,#14894,.F.);
#20321=ORIENTED_EDGE('',*,*,#15047,.F.);
#20322=ORIENTED_EDGE('',*,*,#15052,.T.);
#20323=ORIENTED_EDGE('',*,*,#15053,.F.);
#20324=ORIENTED_EDGE('',*,*,#15048,.F.);
#20325=ORIENTED_EDGE('',*,*,#15054,.T.);
#20326=ORIENTED_EDGE('',*,*,#14873,.T.);
#20327=ORIENTED_EDGE('',*,*,#15055,.T.);
#20328=ORIENTED_EDGE('',*,*,#15056,.T.);
#20329=ORIENTED_EDGE('',*,*,#15057,.T.);
#20330=ORIENTED_EDGE('',*,*,#15058,.T.);
#20331=ORIENTED_EDGE('',*,*,#15054,.F.);
#20332=ORIENTED_EDGE('',*,*,#15059,.T.);
#20333=ORIENTED_EDGE('',*,*,#15060,.F.);
#20334=ORIENTED_EDGE('',*,*,#15061,.F.);
#20335=ORIENTED_EDGE('',*,*,#15062,.F.);
#20336=ORIENTED_EDGE('',*,*,#14874,.F.);
#20337=ORIENTED_EDGE('',*,*,#15058,.F.);
#20338=ORIENTED_EDGE('',*,*,#15063,.T.);
#20339=ORIENTED_EDGE('',*,*,#15064,.F.);
#20340=ORIENTED_EDGE('',*,*,#15059,.F.);
#20341=ORIENTED_EDGE('',*,*,#15065,.T.);
#20342=ORIENTED_EDGE('',*,*,#14853,.T.);
#20343=ORIENTED_EDGE('',*,*,#15066,.T.);
#20344=ORIENTED_EDGE('',*,*,#15067,.T.);
#20345=ORIENTED_EDGE('',*,*,#15068,.T.);
#20346=ORIENTED_EDGE('',*,*,#15069,.T.);
#20347=ORIENTED_EDGE('',*,*,#15065,.F.);
#20348=ORIENTED_EDGE('',*,*,#15070,.T.);
#20349=ORIENTED_EDGE('',*,*,#15071,.F.);
#20350=ORIENTED_EDGE('',*,*,#15072,.F.);
#20351=ORIENTED_EDGE('',*,*,#15073,.F.);
#20352=ORIENTED_EDGE('',*,*,#14854,.F.);
#20353=ORIENTED_EDGE('',*,*,#15069,.F.);
#20354=ORIENTED_EDGE('',*,*,#15074,.T.);
#20355=ORIENTED_EDGE('',*,*,#15075,.F.);
#20356=ORIENTED_EDGE('',*,*,#15070,.F.);
#20357=ORIENTED_EDGE('',*,*,#15076,.T.);
#20358=ORIENTED_EDGE('',*,*,#14833,.T.);
#20359=ORIENTED_EDGE('',*,*,#15077,.T.);
#20360=ORIENTED_EDGE('',*,*,#15078,.T.);
#20361=ORIENTED_EDGE('',*,*,#15079,.T.);
#20362=ORIENTED_EDGE('',*,*,#15080,.T.);
#20363=ORIENTED_EDGE('',*,*,#15076,.F.);
#20364=ORIENTED_EDGE('',*,*,#15081,.T.);
#20365=ORIENTED_EDGE('',*,*,#15082,.F.);
#20366=ORIENTED_EDGE('',*,*,#15083,.F.);
#20367=ORIENTED_EDGE('',*,*,#15084,.F.);
#20368=ORIENTED_EDGE('',*,*,#14834,.F.);
#20369=ORIENTED_EDGE('',*,*,#15080,.F.);
#20370=ORIENTED_EDGE('',*,*,#15085,.T.);
#20371=ORIENTED_EDGE('',*,*,#15086,.F.);
#20372=ORIENTED_EDGE('',*,*,#15081,.F.);
#20373=ORIENTED_EDGE('',*,*,#15087,.T.);
#20374=ORIENTED_EDGE('',*,*,#14813,.T.);
#20375=ORIENTED_EDGE('',*,*,#15088,.T.);
#20376=ORIENTED_EDGE('',*,*,#15089,.T.);
#20377=ORIENTED_EDGE('',*,*,#15090,.T.);
#20378=ORIENTED_EDGE('',*,*,#15091,.T.);
#20379=ORIENTED_EDGE('',*,*,#15087,.F.);
#20380=ORIENTED_EDGE('',*,*,#15092,.T.);
#20381=ORIENTED_EDGE('',*,*,#15093,.F.);
#20382=ORIENTED_EDGE('',*,*,#15094,.F.);
#20383=ORIENTED_EDGE('',*,*,#15095,.F.);
#20384=ORIENTED_EDGE('',*,*,#14814,.F.);
#20385=ORIENTED_EDGE('',*,*,#15091,.F.);
#20386=ORIENTED_EDGE('',*,*,#15096,.T.);
#20387=ORIENTED_EDGE('',*,*,#15097,.F.);
#20388=ORIENTED_EDGE('',*,*,#15092,.F.);
#20389=ORIENTED_EDGE('',*,*,#15098,.T.);
#20390=ORIENTED_EDGE('',*,*,#14793,.T.);
#20391=ORIENTED_EDGE('',*,*,#15099,.T.);
#20392=ORIENTED_EDGE('',*,*,#15100,.T.);
#20393=ORIENTED_EDGE('',*,*,#15101,.T.);
#20394=ORIENTED_EDGE('',*,*,#15102,.T.);
#20395=ORIENTED_EDGE('',*,*,#15098,.F.);
#20396=ORIENTED_EDGE('',*,*,#15103,.T.);
#20397=ORIENTED_EDGE('',*,*,#15104,.F.);
#20398=ORIENTED_EDGE('',*,*,#15105,.F.);
#20399=ORIENTED_EDGE('',*,*,#15106,.F.);
#20400=ORIENTED_EDGE('',*,*,#14794,.F.);
#20401=ORIENTED_EDGE('',*,*,#15102,.F.);
#20402=ORIENTED_EDGE('',*,*,#15107,.T.);
#20403=ORIENTED_EDGE('',*,*,#15108,.F.);
#20404=ORIENTED_EDGE('',*,*,#15103,.F.);
#20405=ORIENTED_EDGE('',*,*,#15109,.T.);
#20406=ORIENTED_EDGE('',*,*,#14773,.T.);
#20407=ORIENTED_EDGE('',*,*,#15110,.T.);
#20408=ORIENTED_EDGE('',*,*,#15111,.T.);
#20409=ORIENTED_EDGE('',*,*,#15112,.T.);
#20410=ORIENTED_EDGE('',*,*,#15113,.T.);
#20411=ORIENTED_EDGE('',*,*,#15109,.F.);
#20412=ORIENTED_EDGE('',*,*,#15114,.T.);
#20413=ORIENTED_EDGE('',*,*,#15115,.F.);
#20414=ORIENTED_EDGE('',*,*,#15116,.F.);
#20415=ORIENTED_EDGE('',*,*,#15117,.F.);
#20416=ORIENTED_EDGE('',*,*,#14774,.F.);
#20417=ORIENTED_EDGE('',*,*,#15113,.F.);
#20418=ORIENTED_EDGE('',*,*,#15118,.T.);
#20419=ORIENTED_EDGE('',*,*,#15119,.F.);
#20420=ORIENTED_EDGE('',*,*,#15114,.F.);
#20421=ORIENTED_EDGE('',*,*,#15120,.T.);
#20422=ORIENTED_EDGE('',*,*,#15121,.T.);
#20423=ORIENTED_EDGE('',*,*,#15122,.T.);
#20424=ORIENTED_EDGE('',*,*,#14770,.T.);
#20425=ORIENTED_EDGE('',*,*,#15123,.T.);
#20426=ORIENTED_EDGE('',*,*,#15124,.T.);
#20427=ORIENTED_EDGE('',*,*,#15121,.F.);
#20428=ORIENTED_EDGE('',*,*,#15125,.T.);
#20429=ORIENTED_EDGE('',*,*,#15126,.F.);
#20430=ORIENTED_EDGE('',*,*,#15127,.F.);
#20431=ORIENTED_EDGE('',*,*,#15120,.F.);
#20432=ORIENTED_EDGE('',*,*,#15128,.T.);
#20433=ORIENTED_EDGE('',*,*,#15129,.F.);
#20434=ORIENTED_EDGE('',*,*,#15125,.F.);
#20435=ORIENTED_EDGE('',*,*,#15130,.T.);
#20436=ORIENTED_EDGE('',*,*,#15131,.T.);
#20437=ORIENTED_EDGE('',*,*,#15132,.T.);
#20438=ORIENTED_EDGE('',*,*,#14990,.T.);
#20439=ORIENTED_EDGE('',*,*,#15133,.T.);
#20440=ORIENTED_EDGE('',*,*,#15134,.T.);
#20441=ORIENTED_EDGE('',*,*,#15131,.F.);
#20442=ORIENTED_EDGE('',*,*,#15135,.T.);
#20443=ORIENTED_EDGE('',*,*,#15136,.F.);
#20444=ORIENTED_EDGE('',*,*,#15137,.F.);
#20445=ORIENTED_EDGE('',*,*,#15130,.F.);
#20446=ORIENTED_EDGE('',*,*,#15138,.T.);
#20447=ORIENTED_EDGE('',*,*,#15139,.F.);
#20448=ORIENTED_EDGE('',*,*,#15135,.F.);
#20449=ORIENTED_EDGE('',*,*,#15140,.T.);
#20450=ORIENTED_EDGE('',*,*,#15141,.T.);
#20451=ORIENTED_EDGE('',*,*,#15142,.T.);
#20452=ORIENTED_EDGE('',*,*,#14970,.T.);
#20453=ORIENTED_EDGE('',*,*,#15143,.T.);
#20454=ORIENTED_EDGE('',*,*,#15144,.T.);
#20455=ORIENTED_EDGE('',*,*,#15141,.F.);
#20456=ORIENTED_EDGE('',*,*,#15145,.T.);
#20457=ORIENTED_EDGE('',*,*,#15146,.F.);
#20458=ORIENTED_EDGE('',*,*,#15147,.F.);
#20459=ORIENTED_EDGE('',*,*,#15140,.F.);
#20460=ORIENTED_EDGE('',*,*,#15148,.T.);
#20461=ORIENTED_EDGE('',*,*,#15149,.F.);
#20462=ORIENTED_EDGE('',*,*,#15145,.F.);
#20463=ORIENTED_EDGE('',*,*,#15150,.T.);
#20464=ORIENTED_EDGE('',*,*,#15151,.T.);
#20465=ORIENTED_EDGE('',*,*,#15152,.T.);
#20466=ORIENTED_EDGE('',*,*,#14950,.T.);
#20467=ORIENTED_EDGE('',*,*,#15153,.T.);
#20468=ORIENTED_EDGE('',*,*,#15154,.T.);
#20469=ORIENTED_EDGE('',*,*,#15151,.F.);
#20470=ORIENTED_EDGE('',*,*,#15155,.T.);
#20471=ORIENTED_EDGE('',*,*,#15156,.F.);
#20472=ORIENTED_EDGE('',*,*,#15157,.F.);
#20473=ORIENTED_EDGE('',*,*,#15150,.F.);
#20474=ORIENTED_EDGE('',*,*,#15158,.T.);
#20475=ORIENTED_EDGE('',*,*,#15159,.F.);
#20476=ORIENTED_EDGE('',*,*,#15155,.F.);
#20477=ORIENTED_EDGE('',*,*,#15160,.T.);
#20478=ORIENTED_EDGE('',*,*,#15161,.T.);
#20479=ORIENTED_EDGE('',*,*,#15162,.T.);
#20480=ORIENTED_EDGE('',*,*,#14930,.T.);
#20481=ORIENTED_EDGE('',*,*,#15163,.T.);
#20482=ORIENTED_EDGE('',*,*,#15164,.T.);
#20483=ORIENTED_EDGE('',*,*,#15161,.F.);
#20484=ORIENTED_EDGE('',*,*,#15165,.T.);
#20485=ORIENTED_EDGE('',*,*,#15166,.F.);
#20486=ORIENTED_EDGE('',*,*,#15167,.F.);
#20487=ORIENTED_EDGE('',*,*,#15160,.F.);
#20488=ORIENTED_EDGE('',*,*,#15168,.T.);
#20489=ORIENTED_EDGE('',*,*,#15169,.F.);
#20490=ORIENTED_EDGE('',*,*,#15165,.F.);
#20491=ORIENTED_EDGE('',*,*,#15170,.T.);
#20492=ORIENTED_EDGE('',*,*,#15171,.T.);
#20493=ORIENTED_EDGE('',*,*,#15172,.T.);
#20494=ORIENTED_EDGE('',*,*,#14910,.T.);
#20495=ORIENTED_EDGE('',*,*,#15173,.T.);
#20496=ORIENTED_EDGE('',*,*,#15174,.T.);
#20497=ORIENTED_EDGE('',*,*,#15171,.F.);
#20498=ORIENTED_EDGE('',*,*,#15175,.T.);
#20499=ORIENTED_EDGE('',*,*,#15176,.F.);
#20500=ORIENTED_EDGE('',*,*,#15177,.F.);
#20501=ORIENTED_EDGE('',*,*,#15170,.F.);
#20502=ORIENTED_EDGE('',*,*,#15178,.T.);
#20503=ORIENTED_EDGE('',*,*,#15179,.F.);
#20504=ORIENTED_EDGE('',*,*,#15175,.F.);
#20505=ORIENTED_EDGE('',*,*,#15180,.T.);
#20506=ORIENTED_EDGE('',*,*,#15181,.T.);
#20507=ORIENTED_EDGE('',*,*,#15182,.T.);
#20508=ORIENTED_EDGE('',*,*,#14890,.T.);
#20509=ORIENTED_EDGE('',*,*,#15183,.T.);
#20510=ORIENTED_EDGE('',*,*,#15184,.T.);
#20511=ORIENTED_EDGE('',*,*,#15181,.F.);
#20512=ORIENTED_EDGE('',*,*,#15185,.T.);
#20513=ORIENTED_EDGE('',*,*,#15186,.F.);
#20514=ORIENTED_EDGE('',*,*,#15187,.F.);
#20515=ORIENTED_EDGE('',*,*,#15180,.F.);
#20516=ORIENTED_EDGE('',*,*,#15188,.T.);
#20517=ORIENTED_EDGE('',*,*,#15189,.F.);
#20518=ORIENTED_EDGE('',*,*,#15185,.F.);
#20519=ORIENTED_EDGE('',*,*,#15190,.T.);
#20520=ORIENTED_EDGE('',*,*,#15191,.T.);
#20521=ORIENTED_EDGE('',*,*,#15192,.T.);
#20522=ORIENTED_EDGE('',*,*,#14870,.T.);
#20523=ORIENTED_EDGE('',*,*,#15193,.T.);
#20524=ORIENTED_EDGE('',*,*,#15194,.T.);
#20525=ORIENTED_EDGE('',*,*,#15191,.F.);
#20526=ORIENTED_EDGE('',*,*,#15195,.T.);
#20527=ORIENTED_EDGE('',*,*,#15196,.F.);
#20528=ORIENTED_EDGE('',*,*,#15197,.F.);
#20529=ORIENTED_EDGE('',*,*,#15190,.F.);
#20530=ORIENTED_EDGE('',*,*,#15198,.T.);
#20531=ORIENTED_EDGE('',*,*,#15199,.F.);
#20532=ORIENTED_EDGE('',*,*,#15195,.F.);
#20533=ORIENTED_EDGE('',*,*,#15200,.T.);
#20534=ORIENTED_EDGE('',*,*,#15201,.T.);
#20535=ORIENTED_EDGE('',*,*,#15202,.T.);
#20536=ORIENTED_EDGE('',*,*,#14850,.T.);
#20537=ORIENTED_EDGE('',*,*,#15203,.T.);
#20538=ORIENTED_EDGE('',*,*,#15204,.T.);
#20539=ORIENTED_EDGE('',*,*,#15201,.F.);
#20540=ORIENTED_EDGE('',*,*,#15205,.T.);
#20541=ORIENTED_EDGE('',*,*,#15206,.F.);
#20542=ORIENTED_EDGE('',*,*,#15207,.F.);
#20543=ORIENTED_EDGE('',*,*,#15200,.F.);
#20544=ORIENTED_EDGE('',*,*,#15208,.T.);
#20545=ORIENTED_EDGE('',*,*,#15209,.F.);
#20546=ORIENTED_EDGE('',*,*,#15205,.F.);
#20547=ORIENTED_EDGE('',*,*,#15210,.T.);
#20548=ORIENTED_EDGE('',*,*,#15211,.T.);
#20549=ORIENTED_EDGE('',*,*,#15212,.T.);
#20550=ORIENTED_EDGE('',*,*,#14830,.T.);
#20551=ORIENTED_EDGE('',*,*,#15213,.T.);
#20552=ORIENTED_EDGE('',*,*,#15214,.T.);
#20553=ORIENTED_EDGE('',*,*,#15211,.F.);
#20554=ORIENTED_EDGE('',*,*,#15215,.T.);
#20555=ORIENTED_EDGE('',*,*,#15216,.F.);
#20556=ORIENTED_EDGE('',*,*,#15217,.F.);
#20557=ORIENTED_EDGE('',*,*,#15210,.F.);
#20558=ORIENTED_EDGE('',*,*,#15218,.T.);
#20559=ORIENTED_EDGE('',*,*,#15219,.F.);
#20560=ORIENTED_EDGE('',*,*,#15215,.F.);
#20561=ORIENTED_EDGE('',*,*,#15220,.T.);
#20562=ORIENTED_EDGE('',*,*,#15221,.T.);
#20563=ORIENTED_EDGE('',*,*,#15222,.T.);
#20564=ORIENTED_EDGE('',*,*,#14810,.T.);
#20565=ORIENTED_EDGE('',*,*,#15223,.T.);
#20566=ORIENTED_EDGE('',*,*,#15224,.T.);
#20567=ORIENTED_EDGE('',*,*,#15221,.F.);
#20568=ORIENTED_EDGE('',*,*,#15225,.T.);
#20569=ORIENTED_EDGE('',*,*,#15226,.F.);
#20570=ORIENTED_EDGE('',*,*,#15227,.F.);
#20571=ORIENTED_EDGE('',*,*,#15220,.F.);
#20572=ORIENTED_EDGE('',*,*,#15228,.T.);
#20573=ORIENTED_EDGE('',*,*,#15229,.F.);
#20574=ORIENTED_EDGE('',*,*,#15225,.F.);
#20575=ORIENTED_EDGE('',*,*,#15230,.T.);
#20576=ORIENTED_EDGE('',*,*,#15231,.T.);
#20577=ORIENTED_EDGE('',*,*,#15232,.T.);
#20578=ORIENTED_EDGE('',*,*,#14790,.T.);
#20579=ORIENTED_EDGE('',*,*,#15233,.T.);
#20580=ORIENTED_EDGE('',*,*,#15234,.T.);
#20581=ORIENTED_EDGE('',*,*,#15231,.F.);
#20582=ORIENTED_EDGE('',*,*,#15235,.T.);
#20583=ORIENTED_EDGE('',*,*,#15236,.F.);
#20584=ORIENTED_EDGE('',*,*,#15237,.F.);
#20585=ORIENTED_EDGE('',*,*,#15230,.F.);
#20586=ORIENTED_EDGE('',*,*,#15238,.T.);
#20587=ORIENTED_EDGE('',*,*,#15239,.F.);
#20588=ORIENTED_EDGE('',*,*,#15235,.F.);
#20589=ORIENTED_EDGE('',*,*,#15240,.T.);
#20590=ORIENTED_EDGE('',*,*,#15241,.T.);
#20591=ORIENTED_EDGE('',*,*,#15242,.T.);
#20592=ORIENTED_EDGE('',*,*,#15243,.T.);
#20593=ORIENTED_EDGE('',*,*,#15115,.T.);
#20594=ORIENTED_EDGE('',*,*,#15119,.T.);
#20595=ORIENTED_EDGE('',*,*,#15243,.F.);
#20596=ORIENTED_EDGE('',*,*,#15244,.T.);
#20597=ORIENTED_EDGE('',*,*,#15245,.T.);
#20598=ORIENTED_EDGE('',*,*,#15246,.F.);
#20599=ORIENTED_EDGE('',*,*,#15247,.T.);
#20600=ORIENTED_EDGE('',*,*,#15248,.T.);
#20601=ORIENTED_EDGE('',*,*,#15249,.T.);
#20602=ORIENTED_EDGE('',*,*,#15250,.T.);
#20603=ORIENTED_EDGE('',*,*,#15251,.T.);
#20604=ORIENTED_EDGE('',*,*,#15252,.T.);
#20605=ORIENTED_EDGE('',*,*,#15253,.T.);
#20606=ORIENTED_EDGE('',*,*,#15254,.T.);
#20607=ORIENTED_EDGE('',*,*,#15255,.T.);
#20608=ORIENTED_EDGE('',*,*,#15256,.T.);
#20609=ORIENTED_EDGE('',*,*,#15257,.T.);
#20610=ORIENTED_EDGE('',*,*,#15258,.T.);
#20611=ORIENTED_EDGE('',*,*,#15259,.T.);
#20612=ORIENTED_EDGE('',*,*,#15260,.T.);
#20613=ORIENTED_EDGE('',*,*,#15261,.T.);
#20614=ORIENTED_EDGE('',*,*,#14995,.T.);
#20615=ORIENTED_EDGE('',*,*,#15262,.F.);
#20616=ORIENTED_EDGE('',*,*,#15263,.T.);
#20617=ORIENTED_EDGE('',*,*,#15264,.T.);
#20618=ORIENTED_EDGE('',*,*,#15265,.F.);
#20619=ORIENTED_EDGE('',*,*,#15266,.T.);
#20620=ORIENTED_EDGE('',*,*,#15267,.T.);
#20621=ORIENTED_EDGE('',*,*,#15268,.T.);
#20622=ORIENTED_EDGE('',*,*,#15269,.T.);
#20623=ORIENTED_EDGE('',*,*,#15270,.T.);
#20624=ORIENTED_EDGE('',*,*,#15271,.T.);
#20625=ORIENTED_EDGE('',*,*,#15272,.T.);
#20626=ORIENTED_EDGE('',*,*,#15273,.T.);
#20627=ORIENTED_EDGE('',*,*,#15274,.T.);
#20628=ORIENTED_EDGE('',*,*,#15275,.T.);
#20629=ORIENTED_EDGE('',*,*,#15276,.T.);
#20630=ORIENTED_EDGE('',*,*,#15277,.T.);
#20631=ORIENTED_EDGE('',*,*,#15278,.T.);
#20632=ORIENTED_EDGE('',*,*,#15279,.T.);
#20633=ORIENTED_EDGE('',*,*,#15280,.T.);
#20634=ORIENTED_EDGE('',*,*,#15006,.T.);
#20635=ORIENTED_EDGE('',*,*,#15281,.F.);
#20636=ORIENTED_EDGE('',*,*,#15282,.T.);
#20637=ORIENTED_EDGE('',*,*,#15283,.T.);
#20638=ORIENTED_EDGE('',*,*,#15284,.F.);
#20639=ORIENTED_EDGE('',*,*,#15285,.T.);
#20640=ORIENTED_EDGE('',*,*,#15286,.T.);
#20641=ORIENTED_EDGE('',*,*,#15287,.T.);
#20642=ORIENTED_EDGE('',*,*,#15288,.T.);
#20643=ORIENTED_EDGE('',*,*,#15289,.T.);
#20644=ORIENTED_EDGE('',*,*,#15290,.T.);
#20645=ORIENTED_EDGE('',*,*,#15291,.T.);
#20646=ORIENTED_EDGE('',*,*,#15292,.T.);
#20647=ORIENTED_EDGE('',*,*,#15293,.T.);
#20648=ORIENTED_EDGE('',*,*,#15294,.T.);
#20649=ORIENTED_EDGE('',*,*,#15295,.T.);
#20650=ORIENTED_EDGE('',*,*,#15296,.T.);
#20651=ORIENTED_EDGE('',*,*,#15297,.T.);
#20652=ORIENTED_EDGE('',*,*,#15298,.T.);
#20653=ORIENTED_EDGE('',*,*,#15299,.T.);
#20654=ORIENTED_EDGE('',*,*,#15017,.T.);
#20655=ORIENTED_EDGE('',*,*,#15300,.F.);
#20656=ORIENTED_EDGE('',*,*,#15301,.T.);
#20657=ORIENTED_EDGE('',*,*,#15302,.T.);
#20658=ORIENTED_EDGE('',*,*,#15303,.F.);
#20659=ORIENTED_EDGE('',*,*,#15304,.T.);
#20660=ORIENTED_EDGE('',*,*,#15305,.T.);
#20661=ORIENTED_EDGE('',*,*,#15306,.T.);
#20662=ORIENTED_EDGE('',*,*,#15307,.T.);
#20663=ORIENTED_EDGE('',*,*,#15308,.T.);
#20664=ORIENTED_EDGE('',*,*,#15309,.T.);
#20665=ORIENTED_EDGE('',*,*,#15310,.T.);
#20666=ORIENTED_EDGE('',*,*,#15311,.T.);
#20667=ORIENTED_EDGE('',*,*,#15312,.T.);
#20668=ORIENTED_EDGE('',*,*,#15313,.T.);
#20669=ORIENTED_EDGE('',*,*,#15314,.T.);
#20670=ORIENTED_EDGE('',*,*,#15315,.T.);
#20671=ORIENTED_EDGE('',*,*,#15316,.T.);
#20672=ORIENTED_EDGE('',*,*,#15317,.T.);
#20673=ORIENTED_EDGE('',*,*,#15318,.T.);
#20674=ORIENTED_EDGE('',*,*,#15028,.T.);
#20675=ORIENTED_EDGE('',*,*,#15319,.F.);
#20676=ORIENTED_EDGE('',*,*,#15320,.T.);
#20677=ORIENTED_EDGE('',*,*,#15321,.T.);
#20678=ORIENTED_EDGE('',*,*,#15322,.F.);
#20679=ORIENTED_EDGE('',*,*,#15323,.T.);
#20680=ORIENTED_EDGE('',*,*,#15324,.T.);
#20681=ORIENTED_EDGE('',*,*,#15325,.T.);
#20682=ORIENTED_EDGE('',*,*,#15326,.T.);
#20683=ORIENTED_EDGE('',*,*,#15327,.T.);
#20684=ORIENTED_EDGE('',*,*,#15328,.T.);
#20685=ORIENTED_EDGE('',*,*,#15329,.T.);
#20686=ORIENTED_EDGE('',*,*,#15330,.T.);
#20687=ORIENTED_EDGE('',*,*,#15331,.T.);
#20688=ORIENTED_EDGE('',*,*,#15332,.T.);
#20689=ORIENTED_EDGE('',*,*,#15333,.T.);
#20690=ORIENTED_EDGE('',*,*,#15334,.T.);
#20691=ORIENTED_EDGE('',*,*,#15335,.T.);
#20692=ORIENTED_EDGE('',*,*,#15336,.T.);
#20693=ORIENTED_EDGE('',*,*,#15337,.T.);
#20694=ORIENTED_EDGE('',*,*,#15039,.T.);
#20695=ORIENTED_EDGE('',*,*,#15338,.F.);
#20696=ORIENTED_EDGE('',*,*,#15339,.T.);
#20697=ORIENTED_EDGE('',*,*,#15340,.T.);
#20698=ORIENTED_EDGE('',*,*,#15341,.F.);
#20699=ORIENTED_EDGE('',*,*,#15342,.T.);
#20700=ORIENTED_EDGE('',*,*,#15343,.T.);
#20701=ORIENTED_EDGE('',*,*,#15344,.T.);
#20702=ORIENTED_EDGE('',*,*,#15345,.T.);
#20703=ORIENTED_EDGE('',*,*,#15346,.T.);
#20704=ORIENTED_EDGE('',*,*,#15347,.T.);
#20705=ORIENTED_EDGE('',*,*,#15348,.T.);
#20706=ORIENTED_EDGE('',*,*,#15349,.T.);
#20707=ORIENTED_EDGE('',*,*,#15350,.T.);
#20708=ORIENTED_EDGE('',*,*,#15351,.T.);
#20709=ORIENTED_EDGE('',*,*,#15352,.T.);
#20710=ORIENTED_EDGE('',*,*,#15353,.T.);
#20711=ORIENTED_EDGE('',*,*,#15354,.T.);
#20712=ORIENTED_EDGE('',*,*,#15355,.T.);
#20713=ORIENTED_EDGE('',*,*,#15356,.T.);
#20714=ORIENTED_EDGE('',*,*,#15050,.T.);
#20715=ORIENTED_EDGE('',*,*,#15357,.F.);
#20716=ORIENTED_EDGE('',*,*,#15358,.T.);
#20717=ORIENTED_EDGE('',*,*,#15359,.T.);
#20718=ORIENTED_EDGE('',*,*,#15360,.F.);
#20719=ORIENTED_EDGE('',*,*,#15361,.T.);
#20720=ORIENTED_EDGE('',*,*,#15362,.T.);
#20721=ORIENTED_EDGE('',*,*,#15363,.T.);
#20722=ORIENTED_EDGE('',*,*,#15364,.T.);
#20723=ORIENTED_EDGE('',*,*,#15365,.T.);
#20724=ORIENTED_EDGE('',*,*,#15366,.T.);
#20725=ORIENTED_EDGE('',*,*,#15367,.T.);
#20726=ORIENTED_EDGE('',*,*,#15368,.T.);
#20727=ORIENTED_EDGE('',*,*,#15369,.T.);
#20728=ORIENTED_EDGE('',*,*,#15370,.T.);
#20729=ORIENTED_EDGE('',*,*,#15371,.T.);
#20730=ORIENTED_EDGE('',*,*,#15372,.T.);
#20731=ORIENTED_EDGE('',*,*,#15373,.T.);
#20732=ORIENTED_EDGE('',*,*,#15374,.T.);
#20733=ORIENTED_EDGE('',*,*,#15375,.T.);
#20734=ORIENTED_EDGE('',*,*,#15061,.T.);
#20735=ORIENTED_EDGE('',*,*,#15376,.F.);
#20736=ORIENTED_EDGE('',*,*,#15377,.T.);
#20737=ORIENTED_EDGE('',*,*,#15378,.T.);
#20738=ORIENTED_EDGE('',*,*,#15379,.F.);
#20739=ORIENTED_EDGE('',*,*,#15380,.T.);
#20740=ORIENTED_EDGE('',*,*,#15381,.T.);
#20741=ORIENTED_EDGE('',*,*,#15382,.T.);
#20742=ORIENTED_EDGE('',*,*,#15383,.T.);
#20743=ORIENTED_EDGE('',*,*,#15384,.T.);
#20744=ORIENTED_EDGE('',*,*,#15385,.T.);
#20745=ORIENTED_EDGE('',*,*,#15386,.T.);
#20746=ORIENTED_EDGE('',*,*,#15387,.T.);
#20747=ORIENTED_EDGE('',*,*,#15388,.T.);
#20748=ORIENTED_EDGE('',*,*,#15389,.T.);
#20749=ORIENTED_EDGE('',*,*,#15390,.T.);
#20750=ORIENTED_EDGE('',*,*,#15391,.T.);
#20751=ORIENTED_EDGE('',*,*,#15392,.T.);
#20752=ORIENTED_EDGE('',*,*,#15393,.T.);
#20753=ORIENTED_EDGE('',*,*,#15394,.T.);
#20754=ORIENTED_EDGE('',*,*,#15072,.T.);
#20755=ORIENTED_EDGE('',*,*,#15395,.F.);
#20756=ORIENTED_EDGE('',*,*,#15396,.T.);
#20757=ORIENTED_EDGE('',*,*,#15397,.T.);
#20758=ORIENTED_EDGE('',*,*,#15398,.F.);
#20759=ORIENTED_EDGE('',*,*,#15399,.T.);
#20760=ORIENTED_EDGE('',*,*,#15400,.T.);
#20761=ORIENTED_EDGE('',*,*,#15401,.T.);
#20762=ORIENTED_EDGE('',*,*,#15402,.T.);
#20763=ORIENTED_EDGE('',*,*,#15403,.T.);
#20764=ORIENTED_EDGE('',*,*,#15404,.T.);
#20765=ORIENTED_EDGE('',*,*,#15405,.T.);
#20766=ORIENTED_EDGE('',*,*,#15406,.T.);
#20767=ORIENTED_EDGE('',*,*,#15407,.T.);
#20768=ORIENTED_EDGE('',*,*,#15408,.T.);
#20769=ORIENTED_EDGE('',*,*,#15409,.T.);
#20770=ORIENTED_EDGE('',*,*,#15410,.T.);
#20771=ORIENTED_EDGE('',*,*,#15411,.T.);
#20772=ORIENTED_EDGE('',*,*,#15412,.T.);
#20773=ORIENTED_EDGE('',*,*,#15413,.T.);
#20774=ORIENTED_EDGE('',*,*,#15083,.T.);
#20775=ORIENTED_EDGE('',*,*,#15414,.F.);
#20776=ORIENTED_EDGE('',*,*,#15415,.T.);
#20777=ORIENTED_EDGE('',*,*,#15416,.T.);
#20778=ORIENTED_EDGE('',*,*,#15417,.F.);
#20779=ORIENTED_EDGE('',*,*,#15418,.T.);
#20780=ORIENTED_EDGE('',*,*,#15419,.T.);
#20781=ORIENTED_EDGE('',*,*,#15420,.T.);
#20782=ORIENTED_EDGE('',*,*,#15421,.T.);
#20783=ORIENTED_EDGE('',*,*,#15422,.T.);
#20784=ORIENTED_EDGE('',*,*,#15423,.T.);
#20785=ORIENTED_EDGE('',*,*,#15424,.T.);
#20786=ORIENTED_EDGE('',*,*,#15425,.T.);
#20787=ORIENTED_EDGE('',*,*,#15426,.T.);
#20788=ORIENTED_EDGE('',*,*,#15427,.T.);
#20789=ORIENTED_EDGE('',*,*,#15428,.T.);
#20790=ORIENTED_EDGE('',*,*,#15429,.T.);
#20791=ORIENTED_EDGE('',*,*,#15430,.T.);
#20792=ORIENTED_EDGE('',*,*,#15431,.T.);
#20793=ORIENTED_EDGE('',*,*,#15432,.T.);
#20794=ORIENTED_EDGE('',*,*,#15094,.T.);
#20795=ORIENTED_EDGE('',*,*,#15433,.F.);
#20796=ORIENTED_EDGE('',*,*,#15434,.T.);
#20797=ORIENTED_EDGE('',*,*,#15435,.T.);
#20798=ORIENTED_EDGE('',*,*,#15436,.F.);
#20799=ORIENTED_EDGE('',*,*,#15437,.T.);
#20800=ORIENTED_EDGE('',*,*,#15438,.T.);
#20801=ORIENTED_EDGE('',*,*,#15439,.T.);
#20802=ORIENTED_EDGE('',*,*,#15440,.T.);
#20803=ORIENTED_EDGE('',*,*,#15441,.T.);
#20804=ORIENTED_EDGE('',*,*,#15442,.T.);
#20805=ORIENTED_EDGE('',*,*,#15443,.T.);
#20806=ORIENTED_EDGE('',*,*,#15444,.T.);
#20807=ORIENTED_EDGE('',*,*,#15445,.T.);
#20808=ORIENTED_EDGE('',*,*,#15446,.T.);
#20809=ORIENTED_EDGE('',*,*,#15447,.T.);
#20810=ORIENTED_EDGE('',*,*,#15448,.T.);
#20811=ORIENTED_EDGE('',*,*,#15449,.T.);
#20812=ORIENTED_EDGE('',*,*,#15450,.T.);
#20813=ORIENTED_EDGE('',*,*,#15451,.T.);
#20814=ORIENTED_EDGE('',*,*,#15105,.T.);
#20815=ORIENTED_EDGE('',*,*,#15452,.F.);
#20816=ORIENTED_EDGE('',*,*,#15453,.T.);
#20817=ORIENTED_EDGE('',*,*,#15454,.T.);
#20818=ORIENTED_EDGE('',*,*,#15455,.F.);
#20819=ORIENTED_EDGE('',*,*,#15456,.T.);
#20820=ORIENTED_EDGE('',*,*,#15457,.T.);
#20821=ORIENTED_EDGE('',*,*,#15458,.T.);
#20822=ORIENTED_EDGE('',*,*,#15459,.T.);
#20823=ORIENTED_EDGE('',*,*,#15460,.T.);
#20824=ORIENTED_EDGE('',*,*,#15461,.T.);
#20825=ORIENTED_EDGE('',*,*,#15462,.T.);
#20826=ORIENTED_EDGE('',*,*,#15463,.T.);
#20827=ORIENTED_EDGE('',*,*,#15464,.T.);
#20828=ORIENTED_EDGE('',*,*,#15465,.T.);
#20829=ORIENTED_EDGE('',*,*,#15466,.T.);
#20830=ORIENTED_EDGE('',*,*,#15467,.T.);
#20831=ORIENTED_EDGE('',*,*,#15468,.T.);
#20832=ORIENTED_EDGE('',*,*,#15469,.T.);
#20833=ORIENTED_EDGE('',*,*,#15470,.T.);
#20834=ORIENTED_EDGE('',*,*,#15116,.T.);
#20835=ORIENTED_EDGE('',*,*,#15471,.F.);
#20836=ORIENTED_EDGE('',*,*,#15472,.T.);
#20837=ORIENTED_EDGE('',*,*,#15455,.T.);
#20838=ORIENTED_EDGE('',*,*,#15473,.T.);
#20839=ORIENTED_EDGE('',*,*,#15236,.T.);
#20840=ORIENTED_EDGE('',*,*,#15239,.T.);
#20841=ORIENTED_EDGE('',*,*,#15474,.T.);
#20842=ORIENTED_EDGE('',*,*,#15475,.T.);
#20843=ORIENTED_EDGE('',*,*,#15476,.T.);
#20844=ORIENTED_EDGE('',*,*,#15477,.T.);
#20845=ORIENTED_EDGE('',*,*,#15452,.T.);
#20846=ORIENTED_EDGE('',*,*,#15104,.T.);
#20847=ORIENTED_EDGE('',*,*,#15108,.T.);
#20848=ORIENTED_EDGE('',*,*,#15478,.T.);
#20849=ORIENTED_EDGE('',*,*,#15436,.T.);
#20850=ORIENTED_EDGE('',*,*,#15479,.T.);
#20851=ORIENTED_EDGE('',*,*,#15226,.T.);
#20852=ORIENTED_EDGE('',*,*,#15229,.T.);
#20853=ORIENTED_EDGE('',*,*,#15480,.T.);
#20854=ORIENTED_EDGE('',*,*,#15481,.T.);
#20855=ORIENTED_EDGE('',*,*,#15482,.T.);
#20856=ORIENTED_EDGE('',*,*,#15483,.T.);
#20857=ORIENTED_EDGE('',*,*,#15433,.T.);
#20858=ORIENTED_EDGE('',*,*,#15093,.T.);
#20859=ORIENTED_EDGE('',*,*,#15097,.T.);
#20860=ORIENTED_EDGE('',*,*,#15484,.T.);
#20861=ORIENTED_EDGE('',*,*,#15417,.T.);
#20862=ORIENTED_EDGE('',*,*,#15485,.T.);
#20863=ORIENTED_EDGE('',*,*,#15216,.T.);
#20864=ORIENTED_EDGE('',*,*,#15219,.T.);
#20865=ORIENTED_EDGE('',*,*,#15486,.T.);
#20866=ORIENTED_EDGE('',*,*,#15487,.T.);
#20867=ORIENTED_EDGE('',*,*,#15488,.T.);
#20868=ORIENTED_EDGE('',*,*,#15489,.T.);
#20869=ORIENTED_EDGE('',*,*,#15414,.T.);
#20870=ORIENTED_EDGE('',*,*,#15082,.T.);
#20871=ORIENTED_EDGE('',*,*,#15086,.T.);
#20872=ORIENTED_EDGE('',*,*,#15490,.T.);
#20873=ORIENTED_EDGE('',*,*,#15398,.T.);
#20874=ORIENTED_EDGE('',*,*,#15491,.T.);
#20875=ORIENTED_EDGE('',*,*,#15206,.T.);
#20876=ORIENTED_EDGE('',*,*,#15209,.T.);
#20877=ORIENTED_EDGE('',*,*,#15492,.T.);
#20878=ORIENTED_EDGE('',*,*,#15493,.T.);
#20879=ORIENTED_EDGE('',*,*,#15494,.T.);
#20880=ORIENTED_EDGE('',*,*,#15495,.T.);
#20881=ORIENTED_EDGE('',*,*,#15395,.T.);
#20882=ORIENTED_EDGE('',*,*,#15071,.T.);
#20883=ORIENTED_EDGE('',*,*,#15075,.T.);
#20884=ORIENTED_EDGE('',*,*,#15496,.T.);
#20885=ORIENTED_EDGE('',*,*,#15379,.T.);
#20886=ORIENTED_EDGE('',*,*,#15497,.T.);
#20887=ORIENTED_EDGE('',*,*,#15196,.T.);
#20888=ORIENTED_EDGE('',*,*,#15199,.T.);
#20889=ORIENTED_EDGE('',*,*,#15498,.T.);
#20890=ORIENTED_EDGE('',*,*,#15499,.T.);
#20891=ORIENTED_EDGE('',*,*,#15500,.T.);
#20892=ORIENTED_EDGE('',*,*,#15501,.T.);
#20893=ORIENTED_EDGE('',*,*,#15376,.T.);
#20894=ORIENTED_EDGE('',*,*,#15060,.T.);
#20895=ORIENTED_EDGE('',*,*,#15064,.T.);
#20896=ORIENTED_EDGE('',*,*,#15502,.T.);
#20897=ORIENTED_EDGE('',*,*,#15360,.T.);
#20898=ORIENTED_EDGE('',*,*,#15503,.T.);
#20899=ORIENTED_EDGE('',*,*,#15186,.T.);
#20900=ORIENTED_EDGE('',*,*,#15189,.T.);
#20901=ORIENTED_EDGE('',*,*,#15504,.T.);
#20902=ORIENTED_EDGE('',*,*,#15505,.T.);
#20903=ORIENTED_EDGE('',*,*,#15506,.T.);
#20904=ORIENTED_EDGE('',*,*,#15507,.T.);
#20905=ORIENTED_EDGE('',*,*,#15357,.T.);
#20906=ORIENTED_EDGE('',*,*,#15049,.T.);
#20907=ORIENTED_EDGE('',*,*,#15053,.T.);
#20908=ORIENTED_EDGE('',*,*,#15508,.T.);
#20909=ORIENTED_EDGE('',*,*,#15341,.T.);
#20910=ORIENTED_EDGE('',*,*,#15509,.T.);
#20911=ORIENTED_EDGE('',*,*,#15176,.T.);
#20912=ORIENTED_EDGE('',*,*,#15179,.T.);
#20913=ORIENTED_EDGE('',*,*,#15510,.T.);
#20914=ORIENTED_EDGE('',*,*,#15511,.T.);
#20915=ORIENTED_EDGE('',*,*,#15512,.T.);
#20916=ORIENTED_EDGE('',*,*,#15513,.T.);
#20917=ORIENTED_EDGE('',*,*,#15338,.T.);
#20918=ORIENTED_EDGE('',*,*,#15038,.T.);
#20919=ORIENTED_EDGE('',*,*,#15042,.T.);
#20920=ORIENTED_EDGE('',*,*,#15514,.T.);
#20921=ORIENTED_EDGE('',*,*,#15322,.T.);
#20922=ORIENTED_EDGE('',*,*,#15515,.T.);
#20923=ORIENTED_EDGE('',*,*,#15166,.T.);
#20924=ORIENTED_EDGE('',*,*,#15169,.T.);
#20925=ORIENTED_EDGE('',*,*,#15516,.T.);
#20926=ORIENTED_EDGE('',*,*,#15517,.T.);
#20927=ORIENTED_EDGE('',*,*,#15518,.T.);
#20928=ORIENTED_EDGE('',*,*,#15519,.T.);
#20929=ORIENTED_EDGE('',*,*,#15319,.T.);
#20930=ORIENTED_EDGE('',*,*,#15027,.T.);
#20931=ORIENTED_EDGE('',*,*,#15031,.T.);
#20932=ORIENTED_EDGE('',*,*,#15520,.T.);
#20933=ORIENTED_EDGE('',*,*,#15303,.T.);
#20934=ORIENTED_EDGE('',*,*,#15521,.T.);
#20935=ORIENTED_EDGE('',*,*,#15156,.T.);
#20936=ORIENTED_EDGE('',*,*,#15159,.T.);
#20937=ORIENTED_EDGE('',*,*,#15522,.T.);
#20938=ORIENTED_EDGE('',*,*,#15523,.T.);
#20939=ORIENTED_EDGE('',*,*,#15524,.T.);
#20940=ORIENTED_EDGE('',*,*,#15525,.T.);
#20941=ORIENTED_EDGE('',*,*,#15300,.T.);
#20942=ORIENTED_EDGE('',*,*,#15016,.T.);
#20943=ORIENTED_EDGE('',*,*,#15020,.T.);
#20944=ORIENTED_EDGE('',*,*,#15526,.T.);
#20945=ORIENTED_EDGE('',*,*,#15284,.T.);
#20946=ORIENTED_EDGE('',*,*,#15527,.T.);
#20947=ORIENTED_EDGE('',*,*,#15146,.T.);
#20948=ORIENTED_EDGE('',*,*,#15149,.T.);
#20949=ORIENTED_EDGE('',*,*,#15528,.T.);
#20950=ORIENTED_EDGE('',*,*,#15529,.T.);
#20951=ORIENTED_EDGE('',*,*,#15530,.T.);
#20952=ORIENTED_EDGE('',*,*,#15531,.T.);
#20953=ORIENTED_EDGE('',*,*,#15281,.T.);
#20954=ORIENTED_EDGE('',*,*,#15005,.T.);
#20955=ORIENTED_EDGE('',*,*,#15009,.T.);
#20956=ORIENTED_EDGE('',*,*,#15532,.T.);
#20957=ORIENTED_EDGE('',*,*,#15265,.T.);
#20958=ORIENTED_EDGE('',*,*,#15533,.T.);
#20959=ORIENTED_EDGE('',*,*,#15136,.T.);
#20960=ORIENTED_EDGE('',*,*,#15139,.T.);
#20961=ORIENTED_EDGE('',*,*,#15534,.T.);
#20962=ORIENTED_EDGE('',*,*,#15535,.T.);
#20963=ORIENTED_EDGE('',*,*,#15536,.T.);
#20964=ORIENTED_EDGE('',*,*,#15537,.T.);
#20965=ORIENTED_EDGE('',*,*,#15262,.T.);
#20966=ORIENTED_EDGE('',*,*,#14994,.T.);
#20967=ORIENTED_EDGE('',*,*,#14998,.T.);
#20968=ORIENTED_EDGE('',*,*,#15538,.T.);
#20969=ORIENTED_EDGE('',*,*,#15246,.T.);
#20970=ORIENTED_EDGE('',*,*,#15539,.T.);
#20971=ORIENTED_EDGE('',*,*,#15126,.T.);
#20972=ORIENTED_EDGE('',*,*,#15129,.T.);
#20973=ORIENTED_EDGE('',*,*,#15540,.T.);
#20974=ORIENTED_EDGE('',*,*,#14772,.F.);
#20975=ORIENTED_EDGE('',*,*,#15541,.T.);
#20976=ORIENTED_EDGE('',*,*,#15244,.F.);
#20977=ORIENTED_EDGE('',*,*,#15242,.F.);
#20978=ORIENTED_EDGE('',*,*,#15542,.F.);
#20979=ORIENTED_EDGE('',*,*,#15110,.F.);
#20980=ORIENTED_EDGE('',*,*,#15111,.F.);
#20981=ORIENTED_EDGE('',*,*,#15542,.T.);
#20982=ORIENTED_EDGE('',*,*,#15241,.F.);
#20983=ORIENTED_EDGE('',*,*,#15543,.F.);
#20984=ORIENTED_EDGE('',*,*,#15112,.F.);
#20985=ORIENTED_EDGE('',*,*,#15543,.T.);
#20986=ORIENTED_EDGE('',*,*,#15240,.F.);
#20987=ORIENTED_EDGE('',*,*,#15118,.F.);
#20988=ORIENTED_EDGE('',*,*,#14775,.F.);
#20989=ORIENTED_EDGE('',*,*,#15117,.T.);
#20990=ORIENTED_EDGE('',*,*,#15470,.F.);
#20991=ORIENTED_EDGE('',*,*,#15544,.F.);
#20992=ORIENTED_EDGE('',*,*,#14776,.F.);
#20993=ORIENTED_EDGE('',*,*,#15544,.T.);
#20994=ORIENTED_EDGE('',*,*,#15469,.F.);
#20995=ORIENTED_EDGE('',*,*,#15545,.F.);
#20996=ORIENTED_EDGE('',*,*,#14777,.F.);
#20997=ORIENTED_EDGE('',*,*,#15545,.T.);
#20998=ORIENTED_EDGE('',*,*,#15468,.F.);
#20999=ORIENTED_EDGE('',*,*,#15546,.F.);
#21000=ORIENTED_EDGE('',*,*,#14778,.F.);
#21001=ORIENTED_EDGE('',*,*,#15546,.T.);
#21002=ORIENTED_EDGE('',*,*,#15467,.F.);
#21003=ORIENTED_EDGE('',*,*,#15547,.F.);
#21004=ORIENTED_EDGE('',*,*,#14779,.F.);
#21005=ORIENTED_EDGE('',*,*,#15547,.T.);
#21006=ORIENTED_EDGE('',*,*,#15466,.F.);
#21007=ORIENTED_EDGE('',*,*,#15548,.F.);
#21008=ORIENTED_EDGE('',*,*,#14780,.F.);
#21009=ORIENTED_EDGE('',*,*,#15548,.T.);
#21010=ORIENTED_EDGE('',*,*,#15465,.F.);
#21011=ORIENTED_EDGE('',*,*,#15549,.F.);
#21012=ORIENTED_EDGE('',*,*,#14781,.F.);
#21013=ORIENTED_EDGE('',*,*,#15549,.T.);
#21014=ORIENTED_EDGE('',*,*,#15464,.F.);
#21015=ORIENTED_EDGE('',*,*,#15550,.F.);
#21016=ORIENTED_EDGE('',*,*,#14782,.F.);
#21017=ORIENTED_EDGE('',*,*,#15550,.T.);
#21018=ORIENTED_EDGE('',*,*,#15463,.F.);
#21019=ORIENTED_EDGE('',*,*,#15551,.F.);
#21020=ORIENTED_EDGE('',*,*,#14783,.F.);
#21021=ORIENTED_EDGE('',*,*,#15551,.T.);
#21022=ORIENTED_EDGE('',*,*,#15462,.F.);
#21023=ORIENTED_EDGE('',*,*,#15552,.F.);
#21024=ORIENTED_EDGE('',*,*,#14784,.F.);
#21025=ORIENTED_EDGE('',*,*,#15552,.T.);
#21026=ORIENTED_EDGE('',*,*,#15461,.F.);
#21027=ORIENTED_EDGE('',*,*,#15553,.F.);
#21028=ORIENTED_EDGE('',*,*,#14785,.F.);
#21029=ORIENTED_EDGE('',*,*,#15553,.T.);
#21030=ORIENTED_EDGE('',*,*,#15460,.F.);
#21031=ORIENTED_EDGE('',*,*,#15554,.F.);
#21032=ORIENTED_EDGE('',*,*,#14786,.F.);
#21033=ORIENTED_EDGE('',*,*,#15554,.T.);
#21034=ORIENTED_EDGE('',*,*,#15459,.F.);
#21035=ORIENTED_EDGE('',*,*,#15555,.F.);
#21036=ORIENTED_EDGE('',*,*,#14787,.F.);
#21037=ORIENTED_EDGE('',*,*,#15555,.T.);
#21038=ORIENTED_EDGE('',*,*,#15458,.F.);
#21039=ORIENTED_EDGE('',*,*,#15556,.F.);
#21040=ORIENTED_EDGE('',*,*,#14788,.F.);
#21041=ORIENTED_EDGE('',*,*,#15556,.T.);
#21042=ORIENTED_EDGE('',*,*,#15457,.F.);
#21043=ORIENTED_EDGE('',*,*,#15557,.F.);
#21044=ORIENTED_EDGE('',*,*,#15233,.F.);
#21045=ORIENTED_EDGE('',*,*,#14789,.F.);
#21046=ORIENTED_EDGE('',*,*,#15557,.T.);
#21047=ORIENTED_EDGE('',*,*,#15456,.F.);
#21048=ORIENTED_EDGE('',*,*,#15472,.F.);
#21049=ORIENTED_EDGE('',*,*,#15558,.F.);
#21050=ORIENTED_EDGE('',*,*,#15234,.F.);
#21051=ORIENTED_EDGE('',*,*,#15558,.T.);
#21052=ORIENTED_EDGE('',*,*,#15474,.F.);
#21053=ORIENTED_EDGE('',*,*,#15238,.F.);
#21054=ORIENTED_EDGE('',*,*,#14791,.F.);
#21055=ORIENTED_EDGE('',*,*,#15232,.F.);
#21056=ORIENTED_EDGE('',*,*,#15237,.T.);
#21057=ORIENTED_EDGE('',*,*,#15473,.F.);
#21058=ORIENTED_EDGE('',*,*,#15454,.F.);
#21059=ORIENTED_EDGE('',*,*,#15559,.F.);
#21060=ORIENTED_EDGE('',*,*,#14792,.F.);
#21061=ORIENTED_EDGE('',*,*,#15559,.T.);
#21062=ORIENTED_EDGE('',*,*,#15453,.F.);
#21063=ORIENTED_EDGE('',*,*,#15477,.F.);
#21064=ORIENTED_EDGE('',*,*,#15560,.F.);
#21065=ORIENTED_EDGE('',*,*,#15099,.F.);
#21066=ORIENTED_EDGE('',*,*,#15100,.F.);
#21067=ORIENTED_EDGE('',*,*,#15560,.T.);
#21068=ORIENTED_EDGE('',*,*,#15476,.F.);
#21069=ORIENTED_EDGE('',*,*,#15561,.F.);
#21070=ORIENTED_EDGE('',*,*,#15101,.F.);
#21071=ORIENTED_EDGE('',*,*,#15561,.T.);
#21072=ORIENTED_EDGE('',*,*,#15475,.F.);
#21073=ORIENTED_EDGE('',*,*,#15107,.F.);
#21074=ORIENTED_EDGE('',*,*,#14795,.F.);
#21075=ORIENTED_EDGE('',*,*,#15106,.T.);
#21076=ORIENTED_EDGE('',*,*,#15451,.F.);
#21077=ORIENTED_EDGE('',*,*,#15562,.F.);
#21078=ORIENTED_EDGE('',*,*,#14796,.F.);
#21079=ORIENTED_EDGE('',*,*,#15562,.T.);
#21080=ORIENTED_EDGE('',*,*,#15450,.F.);
#21081=ORIENTED_EDGE('',*,*,#15563,.F.);
#21082=ORIENTED_EDGE('',*,*,#14797,.F.);
#21083=ORIENTED_EDGE('',*,*,#15563,.T.);
#21084=ORIENTED_EDGE('',*,*,#15449,.F.);
#21085=ORIENTED_EDGE('',*,*,#15564,.F.);
#21086=ORIENTED_EDGE('',*,*,#14798,.F.);
#21087=ORIENTED_EDGE('',*,*,#15564,.T.);
#21088=ORIENTED_EDGE('',*,*,#15448,.F.);
#21089=ORIENTED_EDGE('',*,*,#15565,.F.);
#21090=ORIENTED_EDGE('',*,*,#14799,.F.);
#21091=ORIENTED_EDGE('',*,*,#15565,.T.);
#21092=ORIENTED_EDGE('',*,*,#15447,.F.);
#21093=ORIENTED_EDGE('',*,*,#15566,.F.);
#21094=ORIENTED_EDGE('',*,*,#14800,.F.);
#21095=ORIENTED_EDGE('',*,*,#15566,.T.);
#21096=ORIENTED_EDGE('',*,*,#15446,.F.);
#21097=ORIENTED_EDGE('',*,*,#15567,.F.);
#21098=ORIENTED_EDGE('',*,*,#14801,.F.);
#21099=ORIENTED_EDGE('',*,*,#15567,.T.);
#21100=ORIENTED_EDGE('',*,*,#15445,.F.);
#21101=ORIENTED_EDGE('',*,*,#15568,.F.);
#21102=ORIENTED_EDGE('',*,*,#14802,.F.);
#21103=ORIENTED_EDGE('',*,*,#15568,.T.);
#21104=ORIENTED_EDGE('',*,*,#15444,.F.);
#21105=ORIENTED_EDGE('',*,*,#15569,.F.);
#21106=ORIENTED_EDGE('',*,*,#14803,.F.);
#21107=ORIENTED_EDGE('',*,*,#15569,.T.);
#21108=ORIENTED_EDGE('',*,*,#15443,.F.);
#21109=ORIENTED_EDGE('',*,*,#15570,.F.);
#21110=ORIENTED_EDGE('',*,*,#14804,.F.);
#21111=ORIENTED_EDGE('',*,*,#15570,.T.);
#21112=ORIENTED_EDGE('',*,*,#15442,.F.);
#21113=ORIENTED_EDGE('',*,*,#15571,.F.);
#21114=ORIENTED_EDGE('',*,*,#14805,.F.);
#21115=ORIENTED_EDGE('',*,*,#15571,.T.);
#21116=ORIENTED_EDGE('',*,*,#15441,.F.);
#21117=ORIENTED_EDGE('',*,*,#15572,.F.);
#21118=ORIENTED_EDGE('',*,*,#14806,.F.);
#21119=ORIENTED_EDGE('',*,*,#15572,.T.);
#21120=ORIENTED_EDGE('',*,*,#15440,.F.);
#21121=ORIENTED_EDGE('',*,*,#15573,.F.);
#21122=ORIENTED_EDGE('',*,*,#14807,.F.);
#21123=ORIENTED_EDGE('',*,*,#15573,.T.);
#21124=ORIENTED_EDGE('',*,*,#15439,.F.);
#21125=ORIENTED_EDGE('',*,*,#15574,.F.);
#21126=ORIENTED_EDGE('',*,*,#14808,.F.);
#21127=ORIENTED_EDGE('',*,*,#15574,.T.);
#21128=ORIENTED_EDGE('',*,*,#15438,.F.);
#21129=ORIENTED_EDGE('',*,*,#15575,.F.);
#21130=ORIENTED_EDGE('',*,*,#15223,.F.);
#21131=ORIENTED_EDGE('',*,*,#14809,.F.);
#21132=ORIENTED_EDGE('',*,*,#15575,.T.);
#21133=ORIENTED_EDGE('',*,*,#15437,.F.);
#21134=ORIENTED_EDGE('',*,*,#15478,.F.);
#21135=ORIENTED_EDGE('',*,*,#15576,.F.);
#21136=ORIENTED_EDGE('',*,*,#15224,.F.);
#21137=ORIENTED_EDGE('',*,*,#15576,.T.);
#21138=ORIENTED_EDGE('',*,*,#15480,.F.);
#21139=ORIENTED_EDGE('',*,*,#15228,.F.);
#21140=ORIENTED_EDGE('',*,*,#14811,.F.);
#21141=ORIENTED_EDGE('',*,*,#15222,.F.);
#21142=ORIENTED_EDGE('',*,*,#15227,.T.);
#21143=ORIENTED_EDGE('',*,*,#15479,.F.);
#21144=ORIENTED_EDGE('',*,*,#15435,.F.);
#21145=ORIENTED_EDGE('',*,*,#15577,.F.);
#21146=ORIENTED_EDGE('',*,*,#14812,.F.);
#21147=ORIENTED_EDGE('',*,*,#15577,.T.);
#21148=ORIENTED_EDGE('',*,*,#15434,.F.);
#21149=ORIENTED_EDGE('',*,*,#15483,.F.);
#21150=ORIENTED_EDGE('',*,*,#15578,.F.);
#21151=ORIENTED_EDGE('',*,*,#15088,.F.);
#21152=ORIENTED_EDGE('',*,*,#15089,.F.);
#21153=ORIENTED_EDGE('',*,*,#15578,.T.);
#21154=ORIENTED_EDGE('',*,*,#15482,.F.);
#21155=ORIENTED_EDGE('',*,*,#15579,.F.);
#21156=ORIENTED_EDGE('',*,*,#15090,.F.);
#21157=ORIENTED_EDGE('',*,*,#15579,.T.);
#21158=ORIENTED_EDGE('',*,*,#15481,.F.);
#21159=ORIENTED_EDGE('',*,*,#15096,.F.);
#21160=ORIENTED_EDGE('',*,*,#14815,.F.);
#21161=ORIENTED_EDGE('',*,*,#15095,.T.);
#21162=ORIENTED_EDGE('',*,*,#15432,.F.);
#21163=ORIENTED_EDGE('',*,*,#15580,.F.);
#21164=ORIENTED_EDGE('',*,*,#14816,.F.);
#21165=ORIENTED_EDGE('',*,*,#15580,.T.);
#21166=ORIENTED_EDGE('',*,*,#15431,.F.);
#21167=ORIENTED_EDGE('',*,*,#15581,.F.);
#21168=ORIENTED_EDGE('',*,*,#14817,.F.);
#21169=ORIENTED_EDGE('',*,*,#15581,.T.);
#21170=ORIENTED_EDGE('',*,*,#15430,.F.);
#21171=ORIENTED_EDGE('',*,*,#15582,.F.);
#21172=ORIENTED_EDGE('',*,*,#14818,.F.);
#21173=ORIENTED_EDGE('',*,*,#15582,.T.);
#21174=ORIENTED_EDGE('',*,*,#15429,.F.);
#21175=ORIENTED_EDGE('',*,*,#15583,.F.);
#21176=ORIENTED_EDGE('',*,*,#14819,.F.);
#21177=ORIENTED_EDGE('',*,*,#15583,.T.);
#21178=ORIENTED_EDGE('',*,*,#15428,.F.);
#21179=ORIENTED_EDGE('',*,*,#15584,.F.);
#21180=ORIENTED_EDGE('',*,*,#14820,.F.);
#21181=ORIENTED_EDGE('',*,*,#15584,.T.);
#21182=ORIENTED_EDGE('',*,*,#15427,.F.);
#21183=ORIENTED_EDGE('',*,*,#15585,.F.);
#21184=ORIENTED_EDGE('',*,*,#14821,.F.);
#21185=ORIENTED_EDGE('',*,*,#15585,.T.);
#21186=ORIENTED_EDGE('',*,*,#15426,.F.);
#21187=ORIENTED_EDGE('',*,*,#15586,.F.);
#21188=ORIENTED_EDGE('',*,*,#14822,.F.);
#21189=ORIENTED_EDGE('',*,*,#15586,.T.);
#21190=ORIENTED_EDGE('',*,*,#15425,.F.);
#21191=ORIENTED_EDGE('',*,*,#15587,.F.);
#21192=ORIENTED_EDGE('',*,*,#14823,.F.);
#21193=ORIENTED_EDGE('',*,*,#15587,.T.);
#21194=ORIENTED_EDGE('',*,*,#15424,.F.);
#21195=ORIENTED_EDGE('',*,*,#15588,.F.);
#21196=ORIENTED_EDGE('',*,*,#14824,.F.);
#21197=ORIENTED_EDGE('',*,*,#15588,.T.);
#21198=ORIENTED_EDGE('',*,*,#15423,.F.);
#21199=ORIENTED_EDGE('',*,*,#15589,.F.);
#21200=ORIENTED_EDGE('',*,*,#14825,.F.);
#21201=ORIENTED_EDGE('',*,*,#15589,.T.);
#21202=ORIENTED_EDGE('',*,*,#15422,.F.);
#21203=ORIENTED_EDGE('',*,*,#15590,.F.);
#21204=ORIENTED_EDGE('',*,*,#14826,.F.);
#21205=ORIENTED_EDGE('',*,*,#15590,.T.);
#21206=ORIENTED_EDGE('',*,*,#15421,.F.);
#21207=ORIENTED_EDGE('',*,*,#15591,.F.);
#21208=ORIENTED_EDGE('',*,*,#14827,.F.);
#21209=ORIENTED_EDGE('',*,*,#15591,.T.);
#21210=ORIENTED_EDGE('',*,*,#15420,.F.);
#21211=ORIENTED_EDGE('',*,*,#15592,.F.);
#21212=ORIENTED_EDGE('',*,*,#14828,.F.);
#21213=ORIENTED_EDGE('',*,*,#15592,.T.);
#21214=ORIENTED_EDGE('',*,*,#15419,.F.);
#21215=ORIENTED_EDGE('',*,*,#15593,.F.);
#21216=ORIENTED_EDGE('',*,*,#15213,.F.);
#21217=ORIENTED_EDGE('',*,*,#14829,.F.);
#21218=ORIENTED_EDGE('',*,*,#15593,.T.);
#21219=ORIENTED_EDGE('',*,*,#15418,.F.);
#21220=ORIENTED_EDGE('',*,*,#15484,.F.);
#21221=ORIENTED_EDGE('',*,*,#15594,.F.);
#21222=ORIENTED_EDGE('',*,*,#15214,.F.);
#21223=ORIENTED_EDGE('',*,*,#15594,.T.);
#21224=ORIENTED_EDGE('',*,*,#15486,.F.);
#21225=ORIENTED_EDGE('',*,*,#15218,.F.);
#21226=ORIENTED_EDGE('',*,*,#14831,.F.);
#21227=ORIENTED_EDGE('',*,*,#15212,.F.);
#21228=ORIENTED_EDGE('',*,*,#15217,.T.);
#21229=ORIENTED_EDGE('',*,*,#15485,.F.);
#21230=ORIENTED_EDGE('',*,*,#15416,.F.);
#21231=ORIENTED_EDGE('',*,*,#15595,.F.);
#21232=ORIENTED_EDGE('',*,*,#14832,.F.);
#21233=ORIENTED_EDGE('',*,*,#15595,.T.);
#21234=ORIENTED_EDGE('',*,*,#15415,.F.);
#21235=ORIENTED_EDGE('',*,*,#15489,.F.);
#21236=ORIENTED_EDGE('',*,*,#15596,.F.);
#21237=ORIENTED_EDGE('',*,*,#15077,.F.);
#21238=ORIENTED_EDGE('',*,*,#15078,.F.);
#21239=ORIENTED_EDGE('',*,*,#15596,.T.);
#21240=ORIENTED_EDGE('',*,*,#15488,.F.);
#21241=ORIENTED_EDGE('',*,*,#15597,.F.);
#21242=ORIENTED_EDGE('',*,*,#15079,.F.);
#21243=ORIENTED_EDGE('',*,*,#15597,.T.);
#21244=ORIENTED_EDGE('',*,*,#15487,.F.);
#21245=ORIENTED_EDGE('',*,*,#15085,.F.);
#21246=ORIENTED_EDGE('',*,*,#14835,.F.);
#21247=ORIENTED_EDGE('',*,*,#15084,.T.);
#21248=ORIENTED_EDGE('',*,*,#15413,.F.);
#21249=ORIENTED_EDGE('',*,*,#15598,.F.);
#21250=ORIENTED_EDGE('',*,*,#14836,.F.);
#21251=ORIENTED_EDGE('',*,*,#15598,.T.);
#21252=ORIENTED_EDGE('',*,*,#15412,.F.);
#21253=ORIENTED_EDGE('',*,*,#15599,.F.);
#21254=ORIENTED_EDGE('',*,*,#14837,.F.);
#21255=ORIENTED_EDGE('',*,*,#15599,.T.);
#21256=ORIENTED_EDGE('',*,*,#15411,.F.);
#21257=ORIENTED_EDGE('',*,*,#15600,.F.);
#21258=ORIENTED_EDGE('',*,*,#14838,.F.);
#21259=ORIENTED_EDGE('',*,*,#15600,.T.);
#21260=ORIENTED_EDGE('',*,*,#15410,.F.);
#21261=ORIENTED_EDGE('',*,*,#15601,.F.);
#21262=ORIENTED_EDGE('',*,*,#14839,.F.);
#21263=ORIENTED_EDGE('',*,*,#15601,.T.);
#21264=ORIENTED_EDGE('',*,*,#15409,.F.);
#21265=ORIENTED_EDGE('',*,*,#15602,.F.);
#21266=ORIENTED_EDGE('',*,*,#14840,.F.);
#21267=ORIENTED_EDGE('',*,*,#15602,.T.);
#21268=ORIENTED_EDGE('',*,*,#15408,.F.);
#21269=ORIENTED_EDGE('',*,*,#15603,.F.);
#21270=ORIENTED_EDGE('',*,*,#14841,.F.);
#21271=ORIENTED_EDGE('',*,*,#15603,.T.);
#21272=ORIENTED_EDGE('',*,*,#15407,.F.);
#21273=ORIENTED_EDGE('',*,*,#15604,.F.);
#21274=ORIENTED_EDGE('',*,*,#14842,.F.);
#21275=ORIENTED_EDGE('',*,*,#15604,.T.);
#21276=ORIENTED_EDGE('',*,*,#15406,.F.);
#21277=ORIENTED_EDGE('',*,*,#15605,.F.);
#21278=ORIENTED_EDGE('',*,*,#14843,.F.);
#21279=ORIENTED_EDGE('',*,*,#15605,.T.);
#21280=ORIENTED_EDGE('',*,*,#15405,.F.);
#21281=ORIENTED_EDGE('',*,*,#15606,.F.);
#21282=ORIENTED_EDGE('',*,*,#14844,.F.);
#21283=ORIENTED_EDGE('',*,*,#15606,.T.);
#21284=ORIENTED_EDGE('',*,*,#15404,.F.);
#21285=ORIENTED_EDGE('',*,*,#15607,.F.);
#21286=ORIENTED_EDGE('',*,*,#14845,.F.);
#21287=ORIENTED_EDGE('',*,*,#15607,.T.);
#21288=ORIENTED_EDGE('',*,*,#15403,.F.);
#21289=ORIENTED_EDGE('',*,*,#15608,.F.);
#21290=ORIENTED_EDGE('',*,*,#14846,.F.);
#21291=ORIENTED_EDGE('',*,*,#15608,.T.);
#21292=ORIENTED_EDGE('',*,*,#15402,.F.);
#21293=ORIENTED_EDGE('',*,*,#15609,.F.);
#21294=ORIENTED_EDGE('',*,*,#14847,.F.);
#21295=ORIENTED_EDGE('',*,*,#15609,.T.);
#21296=ORIENTED_EDGE('',*,*,#15401,.F.);
#21297=ORIENTED_EDGE('',*,*,#15610,.F.);
#21298=ORIENTED_EDGE('',*,*,#14848,.F.);
#21299=ORIENTED_EDGE('',*,*,#15610,.T.);
#21300=ORIENTED_EDGE('',*,*,#15400,.F.);
#21301=ORIENTED_EDGE('',*,*,#15611,.F.);
#21302=ORIENTED_EDGE('',*,*,#15203,.F.);
#21303=ORIENTED_EDGE('',*,*,#14849,.F.);
#21304=ORIENTED_EDGE('',*,*,#15611,.T.);
#21305=ORIENTED_EDGE('',*,*,#15399,.F.);
#21306=ORIENTED_EDGE('',*,*,#15490,.F.);
#21307=ORIENTED_EDGE('',*,*,#15612,.F.);
#21308=ORIENTED_EDGE('',*,*,#15204,.F.);
#21309=ORIENTED_EDGE('',*,*,#15612,.T.);
#21310=ORIENTED_EDGE('',*,*,#15492,.F.);
#21311=ORIENTED_EDGE('',*,*,#15208,.F.);
#21312=ORIENTED_EDGE('',*,*,#14851,.F.);
#21313=ORIENTED_EDGE('',*,*,#15202,.F.);
#21314=ORIENTED_EDGE('',*,*,#15207,.T.);
#21315=ORIENTED_EDGE('',*,*,#15491,.F.);
#21316=ORIENTED_EDGE('',*,*,#15397,.F.);
#21317=ORIENTED_EDGE('',*,*,#15613,.F.);
#21318=ORIENTED_EDGE('',*,*,#14852,.F.);
#21319=ORIENTED_EDGE('',*,*,#15613,.T.);
#21320=ORIENTED_EDGE('',*,*,#15396,.F.);
#21321=ORIENTED_EDGE('',*,*,#15495,.F.);
#21322=ORIENTED_EDGE('',*,*,#15614,.F.);
#21323=ORIENTED_EDGE('',*,*,#15066,.F.);
#21324=ORIENTED_EDGE('',*,*,#15067,.F.);
#21325=ORIENTED_EDGE('',*,*,#15614,.T.);
#21326=ORIENTED_EDGE('',*,*,#15494,.F.);
#21327=ORIENTED_EDGE('',*,*,#15615,.F.);
#21328=ORIENTED_EDGE('',*,*,#15068,.F.);
#21329=ORIENTED_EDGE('',*,*,#15615,.T.);
#21330=ORIENTED_EDGE('',*,*,#15493,.F.);
#21331=ORIENTED_EDGE('',*,*,#15074,.F.);
#21332=ORIENTED_EDGE('',*,*,#14855,.F.);
#21333=ORIENTED_EDGE('',*,*,#15073,.T.);
#21334=ORIENTED_EDGE('',*,*,#15394,.F.);
#21335=ORIENTED_EDGE('',*,*,#15616,.F.);
#21336=ORIENTED_EDGE('',*,*,#14856,.F.);
#21337=ORIENTED_EDGE('',*,*,#15616,.T.);
#21338=ORIENTED_EDGE('',*,*,#15393,.F.);
#21339=ORIENTED_EDGE('',*,*,#15617,.F.);
#21340=ORIENTED_EDGE('',*,*,#14857,.F.);
#21341=ORIENTED_EDGE('',*,*,#15617,.T.);
#21342=ORIENTED_EDGE('',*,*,#15392,.F.);
#21343=ORIENTED_EDGE('',*,*,#15618,.F.);
#21344=ORIENTED_EDGE('',*,*,#14858,.F.);
#21345=ORIENTED_EDGE('',*,*,#15618,.T.);
#21346=ORIENTED_EDGE('',*,*,#15391,.F.);
#21347=ORIENTED_EDGE('',*,*,#15619,.F.);
#21348=ORIENTED_EDGE('',*,*,#14859,.F.);
#21349=ORIENTED_EDGE('',*,*,#15619,.T.);
#21350=ORIENTED_EDGE('',*,*,#15390,.F.);
#21351=ORIENTED_EDGE('',*,*,#15620,.F.);
#21352=ORIENTED_EDGE('',*,*,#14860,.F.);
#21353=ORIENTED_EDGE('',*,*,#15620,.T.);
#21354=ORIENTED_EDGE('',*,*,#15389,.F.);
#21355=ORIENTED_EDGE('',*,*,#15621,.F.);
#21356=ORIENTED_EDGE('',*,*,#14861,.F.);
#21357=ORIENTED_EDGE('',*,*,#15621,.T.);
#21358=ORIENTED_EDGE('',*,*,#15388,.F.);
#21359=ORIENTED_EDGE('',*,*,#15622,.F.);
#21360=ORIENTED_EDGE('',*,*,#14862,.F.);
#21361=ORIENTED_EDGE('',*,*,#15622,.T.);
#21362=ORIENTED_EDGE('',*,*,#15387,.F.);
#21363=ORIENTED_EDGE('',*,*,#15623,.F.);
#21364=ORIENTED_EDGE('',*,*,#14863,.F.);
#21365=ORIENTED_EDGE('',*,*,#15623,.T.);
#21366=ORIENTED_EDGE('',*,*,#15386,.F.);
#21367=ORIENTED_EDGE('',*,*,#15624,.F.);
#21368=ORIENTED_EDGE('',*,*,#14864,.F.);
#21369=ORIENTED_EDGE('',*,*,#15624,.T.);
#21370=ORIENTED_EDGE('',*,*,#15385,.F.);
#21371=ORIENTED_EDGE('',*,*,#15625,.F.);
#21372=ORIENTED_EDGE('',*,*,#14865,.F.);
#21373=ORIENTED_EDGE('',*,*,#15625,.T.);
#21374=ORIENTED_EDGE('',*,*,#15384,.F.);
#21375=ORIENTED_EDGE('',*,*,#15626,.F.);
#21376=ORIENTED_EDGE('',*,*,#14866,.F.);
#21377=ORIENTED_EDGE('',*,*,#15626,.T.);
#21378=ORIENTED_EDGE('',*,*,#15383,.F.);
#21379=ORIENTED_EDGE('',*,*,#15627,.F.);
#21380=ORIENTED_EDGE('',*,*,#14867,.F.);
#21381=ORIENTED_EDGE('',*,*,#15627,.T.);
#21382=ORIENTED_EDGE('',*,*,#15382,.F.);
#21383=ORIENTED_EDGE('',*,*,#15628,.F.);
#21384=ORIENTED_EDGE('',*,*,#14868,.F.);
#21385=ORIENTED_EDGE('',*,*,#15628,.T.);
#21386=ORIENTED_EDGE('',*,*,#15381,.F.);
#21387=ORIENTED_EDGE('',*,*,#15629,.F.);
#21388=ORIENTED_EDGE('',*,*,#15193,.F.);
#21389=ORIENTED_EDGE('',*,*,#14869,.F.);
#21390=ORIENTED_EDGE('',*,*,#15629,.T.);
#21391=ORIENTED_EDGE('',*,*,#15380,.F.);
#21392=ORIENTED_EDGE('',*,*,#15496,.F.);
#21393=ORIENTED_EDGE('',*,*,#15630,.F.);
#21394=ORIENTED_EDGE('',*,*,#15194,.F.);
#21395=ORIENTED_EDGE('',*,*,#15630,.T.);
#21396=ORIENTED_EDGE('',*,*,#15498,.F.);
#21397=ORIENTED_EDGE('',*,*,#15198,.F.);
#21398=ORIENTED_EDGE('',*,*,#14871,.F.);
#21399=ORIENTED_EDGE('',*,*,#15192,.F.);
#21400=ORIENTED_EDGE('',*,*,#15197,.T.);
#21401=ORIENTED_EDGE('',*,*,#15497,.F.);
#21402=ORIENTED_EDGE('',*,*,#15378,.F.);
#21403=ORIENTED_EDGE('',*,*,#15631,.F.);
#21404=ORIENTED_EDGE('',*,*,#14872,.F.);
#21405=ORIENTED_EDGE('',*,*,#15631,.T.);
#21406=ORIENTED_EDGE('',*,*,#15377,.F.);
#21407=ORIENTED_EDGE('',*,*,#15501,.F.);
#21408=ORIENTED_EDGE('',*,*,#15632,.F.);
#21409=ORIENTED_EDGE('',*,*,#15055,.F.);
#21410=ORIENTED_EDGE('',*,*,#15056,.F.);
#21411=ORIENTED_EDGE('',*,*,#15632,.T.);
#21412=ORIENTED_EDGE('',*,*,#15500,.F.);
#21413=ORIENTED_EDGE('',*,*,#15633,.F.);
#21414=ORIENTED_EDGE('',*,*,#15057,.F.);
#21415=ORIENTED_EDGE('',*,*,#15633,.T.);
#21416=ORIENTED_EDGE('',*,*,#15499,.F.);
#21417=ORIENTED_EDGE('',*,*,#15063,.F.);
#21418=ORIENTED_EDGE('',*,*,#14875,.F.);
#21419=ORIENTED_EDGE('',*,*,#15062,.T.);
#21420=ORIENTED_EDGE('',*,*,#15375,.F.);
#21421=ORIENTED_EDGE('',*,*,#15634,.F.);
#21422=ORIENTED_EDGE('',*,*,#14876,.F.);
#21423=ORIENTED_EDGE('',*,*,#15634,.T.);
#21424=ORIENTED_EDGE('',*,*,#15374,.F.);
#21425=ORIENTED_EDGE('',*,*,#15635,.F.);
#21426=ORIENTED_EDGE('',*,*,#14877,.F.);
#21427=ORIENTED_EDGE('',*,*,#15635,.T.);
#21428=ORIENTED_EDGE('',*,*,#15373,.F.);
#21429=ORIENTED_EDGE('',*,*,#15636,.F.);
#21430=ORIENTED_EDGE('',*,*,#14878,.F.);
#21431=ORIENTED_EDGE('',*,*,#15636,.T.);
#21432=ORIENTED_EDGE('',*,*,#15372,.F.);
#21433=ORIENTED_EDGE('',*,*,#15637,.F.);
#21434=ORIENTED_EDGE('',*,*,#14879,.F.);
#21435=ORIENTED_EDGE('',*,*,#15637,.T.);
#21436=ORIENTED_EDGE('',*,*,#15371,.F.);
#21437=ORIENTED_EDGE('',*,*,#15638,.F.);
#21438=ORIENTED_EDGE('',*,*,#14880,.F.);
#21439=ORIENTED_EDGE('',*,*,#15638,.T.);
#21440=ORIENTED_EDGE('',*,*,#15370,.F.);
#21441=ORIENTED_EDGE('',*,*,#15639,.F.);
#21442=ORIENTED_EDGE('',*,*,#14881,.F.);
#21443=ORIENTED_EDGE('',*,*,#15639,.T.);
#21444=ORIENTED_EDGE('',*,*,#15369,.F.);
#21445=ORIENTED_EDGE('',*,*,#15640,.F.);
#21446=ORIENTED_EDGE('',*,*,#14882,.F.);
#21447=ORIENTED_EDGE('',*,*,#15640,.T.);
#21448=ORIENTED_EDGE('',*,*,#15368,.F.);
#21449=ORIENTED_EDGE('',*,*,#15641,.F.);
#21450=ORIENTED_EDGE('',*,*,#14883,.F.);
#21451=ORIENTED_EDGE('',*,*,#15641,.T.);
#21452=ORIENTED_EDGE('',*,*,#15367,.F.);
#21453=ORIENTED_EDGE('',*,*,#15642,.F.);
#21454=ORIENTED_EDGE('',*,*,#14884,.F.);
#21455=ORIENTED_EDGE('',*,*,#15642,.T.);
#21456=ORIENTED_EDGE('',*,*,#15366,.F.);
#21457=ORIENTED_EDGE('',*,*,#15643,.F.);
#21458=ORIENTED_EDGE('',*,*,#14885,.F.);
#21459=ORIENTED_EDGE('',*,*,#15643,.T.);
#21460=ORIENTED_EDGE('',*,*,#15365,.F.);
#21461=ORIENTED_EDGE('',*,*,#15644,.F.);
#21462=ORIENTED_EDGE('',*,*,#14886,.F.);
#21463=ORIENTED_EDGE('',*,*,#15644,.T.);
#21464=ORIENTED_EDGE('',*,*,#15364,.F.);
#21465=ORIENTED_EDGE('',*,*,#15645,.F.);
#21466=ORIENTED_EDGE('',*,*,#14887,.F.);
#21467=ORIENTED_EDGE('',*,*,#15645,.T.);
#21468=ORIENTED_EDGE('',*,*,#15363,.F.);
#21469=ORIENTED_EDGE('',*,*,#15646,.F.);
#21470=ORIENTED_EDGE('',*,*,#14888,.F.);
#21471=ORIENTED_EDGE('',*,*,#15646,.T.);
#21472=ORIENTED_EDGE('',*,*,#15362,.F.);
#21473=ORIENTED_EDGE('',*,*,#15647,.F.);
#21474=ORIENTED_EDGE('',*,*,#15183,.F.);
#21475=ORIENTED_EDGE('',*,*,#14889,.F.);
#21476=ORIENTED_EDGE('',*,*,#15647,.T.);
#21477=ORIENTED_EDGE('',*,*,#15361,.F.);
#21478=ORIENTED_EDGE('',*,*,#15502,.F.);
#21479=ORIENTED_EDGE('',*,*,#15648,.F.);
#21480=ORIENTED_EDGE('',*,*,#15184,.F.);
#21481=ORIENTED_EDGE('',*,*,#15648,.T.);
#21482=ORIENTED_EDGE('',*,*,#15504,.F.);
#21483=ORIENTED_EDGE('',*,*,#15188,.F.);
#21484=ORIENTED_EDGE('',*,*,#14891,.F.);
#21485=ORIENTED_EDGE('',*,*,#15182,.F.);
#21486=ORIENTED_EDGE('',*,*,#15187,.T.);
#21487=ORIENTED_EDGE('',*,*,#15503,.F.);
#21488=ORIENTED_EDGE('',*,*,#15359,.F.);
#21489=ORIENTED_EDGE('',*,*,#15649,.F.);
#21490=ORIENTED_EDGE('',*,*,#14892,.F.);
#21491=ORIENTED_EDGE('',*,*,#15649,.T.);
#21492=ORIENTED_EDGE('',*,*,#15358,.F.);
#21493=ORIENTED_EDGE('',*,*,#15507,.F.);
#21494=ORIENTED_EDGE('',*,*,#15650,.F.);
#21495=ORIENTED_EDGE('',*,*,#15044,.F.);
#21496=ORIENTED_EDGE('',*,*,#15045,.F.);
#21497=ORIENTED_EDGE('',*,*,#15650,.T.);
#21498=ORIENTED_EDGE('',*,*,#15506,.F.);
#21499=ORIENTED_EDGE('',*,*,#15651,.F.);
#21500=ORIENTED_EDGE('',*,*,#15046,.F.);
#21501=ORIENTED_EDGE('',*,*,#15651,.T.);
#21502=ORIENTED_EDGE('',*,*,#15505,.F.);
#21503=ORIENTED_EDGE('',*,*,#15052,.F.);
#21504=ORIENTED_EDGE('',*,*,#14895,.F.);
#21505=ORIENTED_EDGE('',*,*,#15051,.T.);
#21506=ORIENTED_EDGE('',*,*,#15356,.F.);
#21507=ORIENTED_EDGE('',*,*,#15652,.F.);
#21508=ORIENTED_EDGE('',*,*,#14896,.F.);
#21509=ORIENTED_EDGE('',*,*,#15652,.T.);
#21510=ORIENTED_EDGE('',*,*,#15355,.F.);
#21511=ORIENTED_EDGE('',*,*,#15653,.F.);
#21512=ORIENTED_EDGE('',*,*,#14897,.F.);
#21513=ORIENTED_EDGE('',*,*,#15653,.T.);
#21514=ORIENTED_EDGE('',*,*,#15354,.F.);
#21515=ORIENTED_EDGE('',*,*,#15654,.F.);
#21516=ORIENTED_EDGE('',*,*,#14898,.F.);
#21517=ORIENTED_EDGE('',*,*,#15654,.T.);
#21518=ORIENTED_EDGE('',*,*,#15353,.F.);
#21519=ORIENTED_EDGE('',*,*,#15655,.F.);
#21520=ORIENTED_EDGE('',*,*,#14899,.F.);
#21521=ORIENTED_EDGE('',*,*,#15655,.T.);
#21522=ORIENTED_EDGE('',*,*,#15352,.F.);
#21523=ORIENTED_EDGE('',*,*,#15656,.F.);
#21524=ORIENTED_EDGE('',*,*,#14900,.F.);
#21525=ORIENTED_EDGE('',*,*,#15656,.T.);
#21526=ORIENTED_EDGE('',*,*,#15351,.F.);
#21527=ORIENTED_EDGE('',*,*,#15657,.F.);
#21528=ORIENTED_EDGE('',*,*,#14901,.F.);
#21529=ORIENTED_EDGE('',*,*,#15657,.T.);
#21530=ORIENTED_EDGE('',*,*,#15350,.F.);
#21531=ORIENTED_EDGE('',*,*,#15658,.F.);
#21532=ORIENTED_EDGE('',*,*,#14902,.F.);
#21533=ORIENTED_EDGE('',*,*,#15658,.T.);
#21534=ORIENTED_EDGE('',*,*,#15349,.F.);
#21535=ORIENTED_EDGE('',*,*,#15659,.F.);
#21536=ORIENTED_EDGE('',*,*,#14903,.F.);
#21537=ORIENTED_EDGE('',*,*,#15659,.T.);
#21538=ORIENTED_EDGE('',*,*,#15348,.F.);
#21539=ORIENTED_EDGE('',*,*,#15660,.F.);
#21540=ORIENTED_EDGE('',*,*,#14904,.F.);
#21541=ORIENTED_EDGE('',*,*,#15660,.T.);
#21542=ORIENTED_EDGE('',*,*,#15347,.F.);
#21543=ORIENTED_EDGE('',*,*,#15661,.F.);
#21544=ORIENTED_EDGE('',*,*,#14905,.F.);
#21545=ORIENTED_EDGE('',*,*,#15661,.T.);
#21546=ORIENTED_EDGE('',*,*,#15346,.F.);
#21547=ORIENTED_EDGE('',*,*,#15662,.F.);
#21548=ORIENTED_EDGE('',*,*,#14906,.F.);
#21549=ORIENTED_EDGE('',*,*,#15662,.T.);
#21550=ORIENTED_EDGE('',*,*,#15345,.F.);
#21551=ORIENTED_EDGE('',*,*,#15663,.F.);
#21552=ORIENTED_EDGE('',*,*,#14907,.F.);
#21553=ORIENTED_EDGE('',*,*,#15663,.T.);
#21554=ORIENTED_EDGE('',*,*,#15344,.F.);
#21555=ORIENTED_EDGE('',*,*,#15664,.F.);
#21556=ORIENTED_EDGE('',*,*,#14908,.F.);
#21557=ORIENTED_EDGE('',*,*,#15664,.T.);
#21558=ORIENTED_EDGE('',*,*,#15343,.F.);
#21559=ORIENTED_EDGE('',*,*,#15665,.F.);
#21560=ORIENTED_EDGE('',*,*,#15173,.F.);
#21561=ORIENTED_EDGE('',*,*,#14909,.F.);
#21562=ORIENTED_EDGE('',*,*,#15665,.T.);
#21563=ORIENTED_EDGE('',*,*,#15342,.F.);
#21564=ORIENTED_EDGE('',*,*,#15508,.F.);
#21565=ORIENTED_EDGE('',*,*,#15666,.F.);
#21566=ORIENTED_EDGE('',*,*,#15174,.F.);
#21567=ORIENTED_EDGE('',*,*,#15666,.T.);
#21568=ORIENTED_EDGE('',*,*,#15510,.F.);
#21569=ORIENTED_EDGE('',*,*,#15178,.F.);
#21570=ORIENTED_EDGE('',*,*,#14911,.F.);
#21571=ORIENTED_EDGE('',*,*,#15172,.F.);
#21572=ORIENTED_EDGE('',*,*,#15177,.T.);
#21573=ORIENTED_EDGE('',*,*,#15509,.F.);
#21574=ORIENTED_EDGE('',*,*,#15340,.F.);
#21575=ORIENTED_EDGE('',*,*,#15667,.F.);
#21576=ORIENTED_EDGE('',*,*,#14912,.F.);
#21577=ORIENTED_EDGE('',*,*,#15667,.T.);
#21578=ORIENTED_EDGE('',*,*,#15339,.F.);
#21579=ORIENTED_EDGE('',*,*,#15513,.F.);
#21580=ORIENTED_EDGE('',*,*,#15668,.F.);
#21581=ORIENTED_EDGE('',*,*,#15033,.F.);
#21582=ORIENTED_EDGE('',*,*,#15034,.F.);
#21583=ORIENTED_EDGE('',*,*,#15668,.T.);
#21584=ORIENTED_EDGE('',*,*,#15512,.F.);
#21585=ORIENTED_EDGE('',*,*,#15669,.F.);
#21586=ORIENTED_EDGE('',*,*,#15035,.F.);
#21587=ORIENTED_EDGE('',*,*,#15669,.T.);
#21588=ORIENTED_EDGE('',*,*,#15511,.F.);
#21589=ORIENTED_EDGE('',*,*,#15041,.F.);
#21590=ORIENTED_EDGE('',*,*,#14915,.F.);
#21591=ORIENTED_EDGE('',*,*,#15040,.T.);
#21592=ORIENTED_EDGE('',*,*,#15337,.F.);
#21593=ORIENTED_EDGE('',*,*,#15670,.F.);
#21594=ORIENTED_EDGE('',*,*,#14916,.F.);
#21595=ORIENTED_EDGE('',*,*,#15670,.T.);
#21596=ORIENTED_EDGE('',*,*,#15336,.F.);
#21597=ORIENTED_EDGE('',*,*,#15671,.F.);
#21598=ORIENTED_EDGE('',*,*,#14917,.F.);
#21599=ORIENTED_EDGE('',*,*,#15671,.T.);
#21600=ORIENTED_EDGE('',*,*,#15335,.F.);
#21601=ORIENTED_EDGE('',*,*,#15672,.F.);
#21602=ORIENTED_EDGE('',*,*,#14918,.F.);
#21603=ORIENTED_EDGE('',*,*,#15672,.T.);
#21604=ORIENTED_EDGE('',*,*,#15334,.F.);
#21605=ORIENTED_EDGE('',*,*,#15673,.F.);
#21606=ORIENTED_EDGE('',*,*,#14919,.F.);
#21607=ORIENTED_EDGE('',*,*,#15673,.T.);
#21608=ORIENTED_EDGE('',*,*,#15333,.F.);
#21609=ORIENTED_EDGE('',*,*,#15674,.F.);
#21610=ORIENTED_EDGE('',*,*,#14920,.F.);
#21611=ORIENTED_EDGE('',*,*,#15674,.T.);
#21612=ORIENTED_EDGE('',*,*,#15332,.F.);
#21613=ORIENTED_EDGE('',*,*,#15675,.F.);
#21614=ORIENTED_EDGE('',*,*,#14921,.F.);
#21615=ORIENTED_EDGE('',*,*,#15675,.T.);
#21616=ORIENTED_EDGE('',*,*,#15331,.F.);
#21617=ORIENTED_EDGE('',*,*,#15676,.F.);
#21618=ORIENTED_EDGE('',*,*,#14922,.F.);
#21619=ORIENTED_EDGE('',*,*,#15676,.T.);
#21620=ORIENTED_EDGE('',*,*,#15330,.F.);
#21621=ORIENTED_EDGE('',*,*,#15677,.F.);
#21622=ORIENTED_EDGE('',*,*,#14923,.F.);
#21623=ORIENTED_EDGE('',*,*,#15677,.T.);
#21624=ORIENTED_EDGE('',*,*,#15329,.F.);
#21625=ORIENTED_EDGE('',*,*,#15678,.F.);
#21626=ORIENTED_EDGE('',*,*,#14924,.F.);
#21627=ORIENTED_EDGE('',*,*,#15678,.T.);
#21628=ORIENTED_EDGE('',*,*,#15328,.F.);
#21629=ORIENTED_EDGE('',*,*,#15679,.F.);
#21630=ORIENTED_EDGE('',*,*,#14925,.F.);
#21631=ORIENTED_EDGE('',*,*,#15679,.T.);
#21632=ORIENTED_EDGE('',*,*,#15327,.F.);
#21633=ORIENTED_EDGE('',*,*,#15680,.F.);
#21634=ORIENTED_EDGE('',*,*,#14926,.F.);
#21635=ORIENTED_EDGE('',*,*,#15680,.T.);
#21636=ORIENTED_EDGE('',*,*,#15326,.F.);
#21637=ORIENTED_EDGE('',*,*,#15681,.F.);
#21638=ORIENTED_EDGE('',*,*,#14927,.F.);
#21639=ORIENTED_EDGE('',*,*,#15681,.T.);
#21640=ORIENTED_EDGE('',*,*,#15325,.F.);
#21641=ORIENTED_EDGE('',*,*,#15682,.F.);
#21642=ORIENTED_EDGE('',*,*,#14928,.F.);
#21643=ORIENTED_EDGE('',*,*,#15682,.T.);
#21644=ORIENTED_EDGE('',*,*,#15324,.F.);
#21645=ORIENTED_EDGE('',*,*,#15683,.F.);
#21646=ORIENTED_EDGE('',*,*,#15163,.F.);
#21647=ORIENTED_EDGE('',*,*,#14929,.F.);
#21648=ORIENTED_EDGE('',*,*,#15683,.T.);
#21649=ORIENTED_EDGE('',*,*,#15323,.F.);
#21650=ORIENTED_EDGE('',*,*,#15514,.F.);
#21651=ORIENTED_EDGE('',*,*,#15684,.F.);
#21652=ORIENTED_EDGE('',*,*,#15164,.F.);
#21653=ORIENTED_EDGE('',*,*,#15684,.T.);
#21654=ORIENTED_EDGE('',*,*,#15516,.F.);
#21655=ORIENTED_EDGE('',*,*,#15168,.F.);
#21656=ORIENTED_EDGE('',*,*,#14931,.F.);
#21657=ORIENTED_EDGE('',*,*,#15162,.F.);
#21658=ORIENTED_EDGE('',*,*,#15167,.T.);
#21659=ORIENTED_EDGE('',*,*,#15515,.F.);
#21660=ORIENTED_EDGE('',*,*,#15321,.F.);
#21661=ORIENTED_EDGE('',*,*,#15685,.F.);
#21662=ORIENTED_EDGE('',*,*,#14932,.F.);
#21663=ORIENTED_EDGE('',*,*,#15685,.T.);
#21664=ORIENTED_EDGE('',*,*,#15320,.F.);
#21665=ORIENTED_EDGE('',*,*,#15519,.F.);
#21666=ORIENTED_EDGE('',*,*,#15686,.F.);
#21667=ORIENTED_EDGE('',*,*,#15022,.F.);
#21668=ORIENTED_EDGE('',*,*,#15023,.F.);
#21669=ORIENTED_EDGE('',*,*,#15686,.T.);
#21670=ORIENTED_EDGE('',*,*,#15518,.F.);
#21671=ORIENTED_EDGE('',*,*,#15687,.F.);
#21672=ORIENTED_EDGE('',*,*,#15024,.F.);
#21673=ORIENTED_EDGE('',*,*,#15687,.T.);
#21674=ORIENTED_EDGE('',*,*,#15517,.F.);
#21675=ORIENTED_EDGE('',*,*,#15030,.F.);
#21676=ORIENTED_EDGE('',*,*,#14935,.F.);
#21677=ORIENTED_EDGE('',*,*,#15029,.T.);
#21678=ORIENTED_EDGE('',*,*,#15318,.F.);
#21679=ORIENTED_EDGE('',*,*,#15688,.F.);
#21680=ORIENTED_EDGE('',*,*,#14936,.F.);
#21681=ORIENTED_EDGE('',*,*,#15688,.T.);
#21682=ORIENTED_EDGE('',*,*,#15317,.F.);
#21683=ORIENTED_EDGE('',*,*,#15689,.F.);
#21684=ORIENTED_EDGE('',*,*,#14937,.F.);
#21685=ORIENTED_EDGE('',*,*,#15689,.T.);
#21686=ORIENTED_EDGE('',*,*,#15316,.F.);
#21687=ORIENTED_EDGE('',*,*,#15690,.F.);
#21688=ORIENTED_EDGE('',*,*,#14938,.F.);
#21689=ORIENTED_EDGE('',*,*,#15690,.T.);
#21690=ORIENTED_EDGE('',*,*,#15315,.F.);
#21691=ORIENTED_EDGE('',*,*,#15691,.F.);
#21692=ORIENTED_EDGE('',*,*,#14939,.F.);
#21693=ORIENTED_EDGE('',*,*,#15691,.T.);
#21694=ORIENTED_EDGE('',*,*,#15314,.F.);
#21695=ORIENTED_EDGE('',*,*,#15692,.F.);
#21696=ORIENTED_EDGE('',*,*,#14940,.F.);
#21697=ORIENTED_EDGE('',*,*,#15692,.T.);
#21698=ORIENTED_EDGE('',*,*,#15313,.F.);
#21699=ORIENTED_EDGE('',*,*,#15693,.F.);
#21700=ORIENTED_EDGE('',*,*,#14941,.F.);
#21701=ORIENTED_EDGE('',*,*,#15693,.T.);
#21702=ORIENTED_EDGE('',*,*,#15312,.F.);
#21703=ORIENTED_EDGE('',*,*,#15694,.F.);
#21704=ORIENTED_EDGE('',*,*,#14942,.F.);
#21705=ORIENTED_EDGE('',*,*,#15694,.T.);
#21706=ORIENTED_EDGE('',*,*,#15311,.F.);
#21707=ORIENTED_EDGE('',*,*,#15695,.F.);
#21708=ORIENTED_EDGE('',*,*,#14943,.F.);
#21709=ORIENTED_EDGE('',*,*,#15695,.T.);
#21710=ORIENTED_EDGE('',*,*,#15310,.F.);
#21711=ORIENTED_EDGE('',*,*,#15696,.F.);
#21712=ORIENTED_EDGE('',*,*,#14944,.F.);
#21713=ORIENTED_EDGE('',*,*,#15696,.T.);
#21714=ORIENTED_EDGE('',*,*,#15309,.F.);
#21715=ORIENTED_EDGE('',*,*,#15697,.F.);
#21716=ORIENTED_EDGE('',*,*,#14945,.F.);
#21717=ORIENTED_EDGE('',*,*,#15697,.T.);
#21718=ORIENTED_EDGE('',*,*,#15308,.F.);
#21719=ORIENTED_EDGE('',*,*,#15698,.F.);
#21720=ORIENTED_EDGE('',*,*,#14946,.F.);
#21721=ORIENTED_EDGE('',*,*,#15698,.T.);
#21722=ORIENTED_EDGE('',*,*,#15307,.F.);
#21723=ORIENTED_EDGE('',*,*,#15699,.F.);
#21724=ORIENTED_EDGE('',*,*,#14947,.F.);
#21725=ORIENTED_EDGE('',*,*,#15699,.T.);
#21726=ORIENTED_EDGE('',*,*,#15306,.F.);
#21727=ORIENTED_EDGE('',*,*,#15700,.F.);
#21728=ORIENTED_EDGE('',*,*,#14948,.F.);
#21729=ORIENTED_EDGE('',*,*,#15700,.T.);
#21730=ORIENTED_EDGE('',*,*,#15305,.F.);
#21731=ORIENTED_EDGE('',*,*,#15701,.F.);
#21732=ORIENTED_EDGE('',*,*,#15153,.F.);
#21733=ORIENTED_EDGE('',*,*,#14949,.F.);
#21734=ORIENTED_EDGE('',*,*,#15701,.T.);
#21735=ORIENTED_EDGE('',*,*,#15304,.F.);
#21736=ORIENTED_EDGE('',*,*,#15520,.F.);
#21737=ORIENTED_EDGE('',*,*,#15702,.F.);
#21738=ORIENTED_EDGE('',*,*,#15154,.F.);
#21739=ORIENTED_EDGE('',*,*,#15702,.T.);
#21740=ORIENTED_EDGE('',*,*,#15522,.F.);
#21741=ORIENTED_EDGE('',*,*,#15158,.F.);
#21742=ORIENTED_EDGE('',*,*,#14951,.F.);
#21743=ORIENTED_EDGE('',*,*,#15152,.F.);
#21744=ORIENTED_EDGE('',*,*,#15157,.T.);
#21745=ORIENTED_EDGE('',*,*,#15521,.F.);
#21746=ORIENTED_EDGE('',*,*,#15302,.F.);
#21747=ORIENTED_EDGE('',*,*,#15703,.F.);
#21748=ORIENTED_EDGE('',*,*,#14952,.F.);
#21749=ORIENTED_EDGE('',*,*,#15703,.T.);
#21750=ORIENTED_EDGE('',*,*,#15301,.F.);
#21751=ORIENTED_EDGE('',*,*,#15525,.F.);
#21752=ORIENTED_EDGE('',*,*,#15704,.F.);
#21753=ORIENTED_EDGE('',*,*,#15011,.F.);
#21754=ORIENTED_EDGE('',*,*,#15012,.F.);
#21755=ORIENTED_EDGE('',*,*,#15704,.T.);
#21756=ORIENTED_EDGE('',*,*,#15524,.F.);
#21757=ORIENTED_EDGE('',*,*,#15705,.F.);
#21758=ORIENTED_EDGE('',*,*,#15013,.F.);
#21759=ORIENTED_EDGE('',*,*,#15705,.T.);
#21760=ORIENTED_EDGE('',*,*,#15523,.F.);
#21761=ORIENTED_EDGE('',*,*,#15019,.F.);
#21762=ORIENTED_EDGE('',*,*,#14955,.F.);
#21763=ORIENTED_EDGE('',*,*,#15018,.T.);
#21764=ORIENTED_EDGE('',*,*,#15299,.F.);
#21765=ORIENTED_EDGE('',*,*,#15706,.F.);
#21766=ORIENTED_EDGE('',*,*,#14956,.F.);
#21767=ORIENTED_EDGE('',*,*,#15706,.T.);
#21768=ORIENTED_EDGE('',*,*,#15298,.F.);
#21769=ORIENTED_EDGE('',*,*,#15707,.F.);
#21770=ORIENTED_EDGE('',*,*,#14957,.F.);
#21771=ORIENTED_EDGE('',*,*,#15707,.T.);
#21772=ORIENTED_EDGE('',*,*,#15297,.F.);
#21773=ORIENTED_EDGE('',*,*,#15708,.F.);
#21774=ORIENTED_EDGE('',*,*,#14958,.F.);
#21775=ORIENTED_EDGE('',*,*,#15708,.T.);
#21776=ORIENTED_EDGE('',*,*,#15296,.F.);
#21777=ORIENTED_EDGE('',*,*,#15709,.F.);
#21778=ORIENTED_EDGE('',*,*,#14959,.F.);
#21779=ORIENTED_EDGE('',*,*,#15709,.T.);
#21780=ORIENTED_EDGE('',*,*,#15295,.F.);
#21781=ORIENTED_EDGE('',*,*,#15710,.F.);
#21782=ORIENTED_EDGE('',*,*,#14960,.F.);
#21783=ORIENTED_EDGE('',*,*,#15710,.T.);
#21784=ORIENTED_EDGE('',*,*,#15294,.F.);
#21785=ORIENTED_EDGE('',*,*,#15711,.F.);
#21786=ORIENTED_EDGE('',*,*,#14961,.F.);
#21787=ORIENTED_EDGE('',*,*,#15711,.T.);
#21788=ORIENTED_EDGE('',*,*,#15293,.F.);
#21789=ORIENTED_EDGE('',*,*,#15712,.F.);
#21790=ORIENTED_EDGE('',*,*,#14962,.F.);
#21791=ORIENTED_EDGE('',*,*,#15712,.T.);
#21792=ORIENTED_EDGE('',*,*,#15292,.F.);
#21793=ORIENTED_EDGE('',*,*,#15713,.F.);
#21794=ORIENTED_EDGE('',*,*,#14963,.F.);
#21795=ORIENTED_EDGE('',*,*,#15713,.T.);
#21796=ORIENTED_EDGE('',*,*,#15291,.F.);
#21797=ORIENTED_EDGE('',*,*,#15714,.F.);
#21798=ORIENTED_EDGE('',*,*,#14964,.F.);
#21799=ORIENTED_EDGE('',*,*,#15714,.T.);
#21800=ORIENTED_EDGE('',*,*,#15290,.F.);
#21801=ORIENTED_EDGE('',*,*,#15715,.F.);
#21802=ORIENTED_EDGE('',*,*,#14965,.F.);
#21803=ORIENTED_EDGE('',*,*,#15715,.T.);
#21804=ORIENTED_EDGE('',*,*,#15289,.F.);
#21805=ORIENTED_EDGE('',*,*,#15716,.F.);
#21806=ORIENTED_EDGE('',*,*,#14966,.F.);
#21807=ORIENTED_EDGE('',*,*,#15716,.T.);
#21808=ORIENTED_EDGE('',*,*,#15288,.F.);
#21809=ORIENTED_EDGE('',*,*,#15717,.F.);
#21810=ORIENTED_EDGE('',*,*,#14967,.F.);
#21811=ORIENTED_EDGE('',*,*,#15717,.T.);
#21812=ORIENTED_EDGE('',*,*,#15287,.F.);
#21813=ORIENTED_EDGE('',*,*,#15718,.F.);
#21814=ORIENTED_EDGE('',*,*,#14968,.F.);
#21815=ORIENTED_EDGE('',*,*,#15718,.T.);
#21816=ORIENTED_EDGE('',*,*,#15286,.F.);
#21817=ORIENTED_EDGE('',*,*,#15719,.F.);
#21818=ORIENTED_EDGE('',*,*,#15143,.F.);
#21819=ORIENTED_EDGE('',*,*,#14969,.F.);
#21820=ORIENTED_EDGE('',*,*,#15719,.T.);
#21821=ORIENTED_EDGE('',*,*,#15285,.F.);
#21822=ORIENTED_EDGE('',*,*,#15526,.F.);
#21823=ORIENTED_EDGE('',*,*,#15720,.F.);
#21824=ORIENTED_EDGE('',*,*,#15144,.F.);
#21825=ORIENTED_EDGE('',*,*,#15720,.T.);
#21826=ORIENTED_EDGE('',*,*,#15528,.F.);
#21827=ORIENTED_EDGE('',*,*,#15148,.F.);
#21828=ORIENTED_EDGE('',*,*,#14971,.F.);
#21829=ORIENTED_EDGE('',*,*,#15142,.F.);
#21830=ORIENTED_EDGE('',*,*,#15147,.T.);
#21831=ORIENTED_EDGE('',*,*,#15527,.F.);
#21832=ORIENTED_EDGE('',*,*,#15283,.F.);
#21833=ORIENTED_EDGE('',*,*,#15721,.F.);
#21834=ORIENTED_EDGE('',*,*,#14972,.F.);
#21835=ORIENTED_EDGE('',*,*,#15721,.T.);
#21836=ORIENTED_EDGE('',*,*,#15282,.F.);
#21837=ORIENTED_EDGE('',*,*,#15531,.F.);
#21838=ORIENTED_EDGE('',*,*,#15722,.F.);
#21839=ORIENTED_EDGE('',*,*,#15000,.F.);
#21840=ORIENTED_EDGE('',*,*,#15001,.F.);
#21841=ORIENTED_EDGE('',*,*,#15722,.T.);
#21842=ORIENTED_EDGE('',*,*,#15530,.F.);
#21843=ORIENTED_EDGE('',*,*,#15723,.F.);
#21844=ORIENTED_EDGE('',*,*,#15002,.F.);
#21845=ORIENTED_EDGE('',*,*,#15723,.T.);
#21846=ORIENTED_EDGE('',*,*,#15529,.F.);
#21847=ORIENTED_EDGE('',*,*,#15008,.F.);
#21848=ORIENTED_EDGE('',*,*,#14975,.F.);
#21849=ORIENTED_EDGE('',*,*,#15007,.T.);
#21850=ORIENTED_EDGE('',*,*,#15280,.F.);
#21851=ORIENTED_EDGE('',*,*,#15724,.F.);
#21852=ORIENTED_EDGE('',*,*,#14976,.F.);
#21853=ORIENTED_EDGE('',*,*,#15724,.T.);
#21854=ORIENTED_EDGE('',*,*,#15279,.F.);
#21855=ORIENTED_EDGE('',*,*,#15725,.F.);
#21856=ORIENTED_EDGE('',*,*,#14977,.F.);
#21857=ORIENTED_EDGE('',*,*,#15725,.T.);
#21858=ORIENTED_EDGE('',*,*,#15278,.F.);
#21859=ORIENTED_EDGE('',*,*,#15726,.F.);
#21860=ORIENTED_EDGE('',*,*,#14978,.F.);
#21861=ORIENTED_EDGE('',*,*,#15726,.T.);
#21862=ORIENTED_EDGE('',*,*,#15277,.F.);
#21863=ORIENTED_EDGE('',*,*,#15727,.F.);
#21864=ORIENTED_EDGE('',*,*,#14979,.F.);
#21865=ORIENTED_EDGE('',*,*,#15727,.T.);
#21866=ORIENTED_EDGE('',*,*,#15276,.F.);
#21867=ORIENTED_EDGE('',*,*,#15728,.F.);
#21868=ORIENTED_EDGE('',*,*,#14980,.F.);
#21869=ORIENTED_EDGE('',*,*,#15728,.T.);
#21870=ORIENTED_EDGE('',*,*,#15275,.F.);
#21871=ORIENTED_EDGE('',*,*,#15729,.F.);
#21872=ORIENTED_EDGE('',*,*,#14981,.F.);
#21873=ORIENTED_EDGE('',*,*,#15729,.T.);
#21874=ORIENTED_EDGE('',*,*,#15274,.F.);
#21875=ORIENTED_EDGE('',*,*,#15730,.F.);
#21876=ORIENTED_EDGE('',*,*,#14982,.F.);
#21877=ORIENTED_EDGE('',*,*,#15730,.T.);
#21878=ORIENTED_EDGE('',*,*,#15273,.F.);
#21879=ORIENTED_EDGE('',*,*,#15731,.F.);
#21880=ORIENTED_EDGE('',*,*,#14983,.F.);
#21881=ORIENTED_EDGE('',*,*,#15731,.T.);
#21882=ORIENTED_EDGE('',*,*,#15272,.F.);
#21883=ORIENTED_EDGE('',*,*,#15732,.F.);
#21884=ORIENTED_EDGE('',*,*,#14984,.F.);
#21885=ORIENTED_EDGE('',*,*,#15732,.T.);
#21886=ORIENTED_EDGE('',*,*,#15271,.F.);
#21887=ORIENTED_EDGE('',*,*,#15733,.F.);
#21888=ORIENTED_EDGE('',*,*,#14985,.F.);
#21889=ORIENTED_EDGE('',*,*,#15733,.T.);
#21890=ORIENTED_EDGE('',*,*,#15270,.F.);
#21891=ORIENTED_EDGE('',*,*,#15734,.F.);
#21892=ORIENTED_EDGE('',*,*,#14986,.F.);
#21893=ORIENTED_EDGE('',*,*,#15734,.T.);
#21894=ORIENTED_EDGE('',*,*,#15269,.F.);
#21895=ORIENTED_EDGE('',*,*,#15735,.F.);
#21896=ORIENTED_EDGE('',*,*,#14987,.F.);
#21897=ORIENTED_EDGE('',*,*,#15735,.T.);
#21898=ORIENTED_EDGE('',*,*,#15268,.F.);
#21899=ORIENTED_EDGE('',*,*,#15736,.F.);
#21900=ORIENTED_EDGE('',*,*,#14988,.F.);
#21901=ORIENTED_EDGE('',*,*,#15736,.T.);
#21902=ORIENTED_EDGE('',*,*,#15267,.F.);
#21903=ORIENTED_EDGE('',*,*,#15737,.F.);
#21904=ORIENTED_EDGE('',*,*,#15133,.F.);
#21905=ORIENTED_EDGE('',*,*,#14989,.F.);
#21906=ORIENTED_EDGE('',*,*,#15737,.T.);
#21907=ORIENTED_EDGE('',*,*,#15266,.F.);
#21908=ORIENTED_EDGE('',*,*,#15532,.F.);
#21909=ORIENTED_EDGE('',*,*,#15738,.F.);
#21910=ORIENTED_EDGE('',*,*,#15134,.F.);
#21911=ORIENTED_EDGE('',*,*,#15738,.T.);
#21912=ORIENTED_EDGE('',*,*,#15534,.F.);
#21913=ORIENTED_EDGE('',*,*,#15138,.F.);
#21914=ORIENTED_EDGE('',*,*,#14991,.F.);
#21915=ORIENTED_EDGE('',*,*,#15132,.F.);
#21916=ORIENTED_EDGE('',*,*,#15137,.T.);
#21917=ORIENTED_EDGE('',*,*,#15533,.F.);
#21918=ORIENTED_EDGE('',*,*,#15264,.F.);
#21919=ORIENTED_EDGE('',*,*,#15739,.F.);
#21920=ORIENTED_EDGE('',*,*,#14753,.F.);
#21921=ORIENTED_EDGE('',*,*,#15739,.T.);
#21922=ORIENTED_EDGE('',*,*,#15263,.F.);
#21923=ORIENTED_EDGE('',*,*,#15537,.F.);
#21924=ORIENTED_EDGE('',*,*,#15740,.F.);
#21925=ORIENTED_EDGE('',*,*,#14749,.F.);
#21926=ORIENTED_EDGE('',*,*,#14750,.F.);
#21927=ORIENTED_EDGE('',*,*,#15740,.T.);
#21928=ORIENTED_EDGE('',*,*,#15536,.F.);
#21929=ORIENTED_EDGE('',*,*,#15741,.F.);
#21930=ORIENTED_EDGE('',*,*,#14751,.F.);
#21931=ORIENTED_EDGE('',*,*,#15741,.T.);
#21932=ORIENTED_EDGE('',*,*,#15535,.F.);
#21933=ORIENTED_EDGE('',*,*,#14997,.F.);
#21934=ORIENTED_EDGE('',*,*,#14755,.F.);
#21935=ORIENTED_EDGE('',*,*,#14996,.T.);
#21936=ORIENTED_EDGE('',*,*,#15261,.F.);
#21937=ORIENTED_EDGE('',*,*,#15742,.F.);
#21938=ORIENTED_EDGE('',*,*,#14756,.F.);
#21939=ORIENTED_EDGE('',*,*,#15742,.T.);
#21940=ORIENTED_EDGE('',*,*,#15260,.F.);
#21941=ORIENTED_EDGE('',*,*,#15743,.F.);
#21942=ORIENTED_EDGE('',*,*,#14757,.F.);
#21943=ORIENTED_EDGE('',*,*,#15743,.T.);
#21944=ORIENTED_EDGE('',*,*,#15259,.F.);
#21945=ORIENTED_EDGE('',*,*,#15744,.F.);
#21946=ORIENTED_EDGE('',*,*,#14758,.F.);
#21947=ORIENTED_EDGE('',*,*,#15744,.T.);
#21948=ORIENTED_EDGE('',*,*,#15258,.F.);
#21949=ORIENTED_EDGE('',*,*,#15745,.F.);
#21950=ORIENTED_EDGE('',*,*,#14759,.F.);
#21951=ORIENTED_EDGE('',*,*,#15745,.T.);
#21952=ORIENTED_EDGE('',*,*,#15257,.F.);
#21953=ORIENTED_EDGE('',*,*,#15746,.F.);
#21954=ORIENTED_EDGE('',*,*,#14760,.F.);
#21955=ORIENTED_EDGE('',*,*,#15746,.T.);
#21956=ORIENTED_EDGE('',*,*,#15256,.F.);
#21957=ORIENTED_EDGE('',*,*,#15747,.F.);
#21958=ORIENTED_EDGE('',*,*,#14761,.F.);
#21959=ORIENTED_EDGE('',*,*,#15747,.T.);
#21960=ORIENTED_EDGE('',*,*,#15255,.F.);
#21961=ORIENTED_EDGE('',*,*,#15748,.F.);
#21962=ORIENTED_EDGE('',*,*,#14762,.F.);
#21963=ORIENTED_EDGE('',*,*,#15748,.T.);
#21964=ORIENTED_EDGE('',*,*,#15254,.F.);
#21965=ORIENTED_EDGE('',*,*,#15749,.F.);
#21966=ORIENTED_EDGE('',*,*,#14763,.F.);
#21967=ORIENTED_EDGE('',*,*,#15749,.T.);
#21968=ORIENTED_EDGE('',*,*,#15253,.F.);
#21969=ORIENTED_EDGE('',*,*,#15750,.F.);
#21970=ORIENTED_EDGE('',*,*,#14764,.F.);
#21971=ORIENTED_EDGE('',*,*,#15750,.T.);
#21972=ORIENTED_EDGE('',*,*,#15252,.F.);
#21973=ORIENTED_EDGE('',*,*,#15751,.F.);
#21974=ORIENTED_EDGE('',*,*,#14765,.F.);
#21975=ORIENTED_EDGE('',*,*,#15751,.T.);
#21976=ORIENTED_EDGE('',*,*,#15251,.F.);
#21977=ORIENTED_EDGE('',*,*,#15752,.F.);
#21978=ORIENTED_EDGE('',*,*,#14766,.F.);
#21979=ORIENTED_EDGE('',*,*,#15752,.T.);
#21980=ORIENTED_EDGE('',*,*,#15250,.F.);
#21981=ORIENTED_EDGE('',*,*,#15753,.F.);
#21982=ORIENTED_EDGE('',*,*,#14767,.F.);
#21983=ORIENTED_EDGE('',*,*,#15753,.T.);
#21984=ORIENTED_EDGE('',*,*,#15249,.F.);
#21985=ORIENTED_EDGE('',*,*,#15754,.F.);
#21986=ORIENTED_EDGE('',*,*,#14768,.F.);
#21987=ORIENTED_EDGE('',*,*,#15754,.T.);
#21988=ORIENTED_EDGE('',*,*,#15248,.F.);
#21989=ORIENTED_EDGE('',*,*,#15755,.F.);
#21990=ORIENTED_EDGE('',*,*,#15123,.F.);
#21991=ORIENTED_EDGE('',*,*,#14769,.F.);
#21992=ORIENTED_EDGE('',*,*,#15755,.T.);
#21993=ORIENTED_EDGE('',*,*,#15247,.F.);
#21994=ORIENTED_EDGE('',*,*,#15538,.F.);
#21995=ORIENTED_EDGE('',*,*,#15756,.F.);
#21996=ORIENTED_EDGE('',*,*,#15124,.F.);
#21997=ORIENTED_EDGE('',*,*,#15756,.T.);
#21998=ORIENTED_EDGE('',*,*,#15540,.F.);
#21999=ORIENTED_EDGE('',*,*,#15128,.F.);
#22000=ORIENTED_EDGE('',*,*,#14771,.F.);
#22001=ORIENTED_EDGE('',*,*,#15122,.F.);
#22002=ORIENTED_EDGE('',*,*,#15127,.T.);
#22003=ORIENTED_EDGE('',*,*,#15539,.F.);
#22004=ORIENTED_EDGE('',*,*,#15245,.F.);
#22005=ORIENTED_EDGE('',*,*,#15541,.F.);
#22006=ORIENTED_EDGE('',*,*,#14992,.T.);
#22007=ORIENTED_EDGE('',*,*,#15757,.T.);
#22008=ORIENTED_EDGE('',*,*,#15758,.T.);
#22009=ORIENTED_EDGE('',*,*,#15757,.F.);
#22010=ORIENTED_EDGE('',*,*,#15758,.F.);
#22011=ORIENTED_EDGE('',*,*,#15759,.F.);
#22012=ORIENTED_EDGE('',*,*,#15760,.T.);
#22013=ORIENTED_EDGE('',*,*,#15471,.T.);
#22014=ORIENTED_EDGE('',*,*,#15760,.F.);
#22015=ORIENTED_EDGE('',*,*,#15759,.T.);
#22016=ORIENTED_EDGE('',*,*,#15761,.F.);
#22017=ORIENTED_EDGE('',*,*,#15762,.T.);
#22018=ORIENTED_EDGE('',*,*,#15763,.T.);
#22019=ORIENTED_EDGE('',*,*,#15764,.F.);
#22020=ORIENTED_EDGE('',*,*,#15765,.F.);
#22021=ORIENTED_EDGE('',*,*,#15766,.T.);
#22022=ORIENTED_EDGE('',*,*,#15767,.T.);
#22023=ORIENTED_EDGE('',*,*,#15762,.F.);
#22024=ORIENTED_EDGE('',*,*,#15768,.F.);
#22025=ORIENTED_EDGE('',*,*,#15769,.T.);
#22026=ORIENTED_EDGE('',*,*,#15770,.T.);
#22027=ORIENTED_EDGE('',*,*,#15766,.F.);
#22028=ORIENTED_EDGE('',*,*,#15771,.F.);
#22029=ORIENTED_EDGE('',*,*,#15764,.T.);
#22030=ORIENTED_EDGE('',*,*,#15772,.T.);
#22031=ORIENTED_EDGE('',*,*,#15769,.F.);
#22032=ORIENTED_EDGE('',*,*,#15772,.F.);
#22033=ORIENTED_EDGE('',*,*,#15763,.F.);
#22034=ORIENTED_EDGE('',*,*,#15767,.F.);
#22035=ORIENTED_EDGE('',*,*,#15770,.F.);
#22036=ORIENTED_EDGE('',*,*,#15773,.F.);
#22037=ORIENTED_EDGE('',*,*,#15774,.T.);
#22038=ORIENTED_EDGE('',*,*,#15775,.T.);
#22039=ORIENTED_EDGE('',*,*,#15776,.F.);
#22040=ORIENTED_EDGE('',*,*,#15777,.F.);
#22041=ORIENTED_EDGE('',*,*,#15778,.T.);
#22042=ORIENTED_EDGE('',*,*,#15779,.T.);
#22043=ORIENTED_EDGE('',*,*,#15774,.F.);
#22044=ORIENTED_EDGE('',*,*,#15780,.F.);
#22045=ORIENTED_EDGE('',*,*,#15781,.T.);
#22046=ORIENTED_EDGE('',*,*,#15782,.T.);
#22047=ORIENTED_EDGE('',*,*,#15778,.F.);
#22048=ORIENTED_EDGE('',*,*,#15783,.F.);
#22049=ORIENTED_EDGE('',*,*,#15776,.T.);
#22050=ORIENTED_EDGE('',*,*,#15784,.T.);
#22051=ORIENTED_EDGE('',*,*,#15781,.F.);
#22052=ORIENTED_EDGE('',*,*,#15784,.F.);
#22053=ORIENTED_EDGE('',*,*,#15775,.F.);
#22054=ORIENTED_EDGE('',*,*,#15779,.F.);
#22055=ORIENTED_EDGE('',*,*,#15782,.F.);
#22056=ORIENTED_EDGE('',*,*,#15785,.F.);
#22057=ORIENTED_EDGE('',*,*,#15786,.T.);
#22058=ORIENTED_EDGE('',*,*,#15787,.F.);
#22059=ORIENTED_EDGE('',*,*,#15786,.F.);
#22060=ORIENTED_EDGE('',*,*,#15788,.F.);
#22061=ORIENTED_EDGE('',*,*,#15789,.T.);
#22062=ORIENTED_EDGE('',*,*,#15790,.F.);
#22063=ORIENTED_EDGE('',*,*,#15789,.F.);
#22064=ORIENTED_EDGE('',*,*,#15791,.T.);
#22065=ORIENTED_EDGE('',*,*,#15792,.T.);
#22066=ORIENTED_EDGE('',*,*,#15793,.F.);
#22067=ORIENTED_EDGE('',*,*,#15794,.F.);
#22068=ORIENTED_EDGE('',*,*,#15795,.T.);
#22069=ORIENTED_EDGE('',*,*,#15794,.T.);
#22070=ORIENTED_EDGE('',*,*,#15796,.F.);
#22071=ORIENTED_EDGE('',*,*,#15792,.F.);
#22072=ORIENTED_EDGE('',*,*,#15796,.T.);
#22073=ORIENTED_EDGE('',*,*,#15793,.T.);
#22074=ORIENTED_EDGE('',*,*,#15761,.T.);
#22075=ORIENTED_EDGE('',*,*,#15771,.T.);
#22076=ORIENTED_EDGE('',*,*,#15768,.T.);
#22077=ORIENTED_EDGE('',*,*,#15765,.T.);
#22078=ORIENTED_EDGE('',*,*,#15773,.T.);
#22079=ORIENTED_EDGE('',*,*,#15783,.T.);
#22080=ORIENTED_EDGE('',*,*,#15780,.T.);
#22081=ORIENTED_EDGE('',*,*,#15777,.T.);
#22082=ORIENTED_EDGE('',*,*,#15787,.T.);
#22083=ORIENTED_EDGE('',*,*,#15790,.T.);
#22084=ORIENTED_EDGE('',*,*,#15795,.F.);
#22085=ORIENTED_EDGE('',*,*,#15791,.F.);
#22086=ORIENTED_EDGE('',*,*,#15785,.T.);
#22087=ORIENTED_EDGE('',*,*,#15788,.T.);
#22088=ORIENTED_EDGE('',*,*,#15797,.T.);
#22089=ORIENTED_EDGE('',*,*,#15798,.T.);
#22090=ORIENTED_EDGE('',*,*,#15799,.T.);
#22091=ORIENTED_EDGE('',*,*,#15800,.T.);
#22092=ORIENTED_EDGE('',*,*,#15799,.F.);
#22093=ORIENTED_EDGE('',*,*,#15800,.F.);
#22094=ORIENTED_EDGE('',*,*,#15801,.T.);
#22095=ORIENTED_EDGE('',*,*,#15802,.F.);
#22096=ORIENTED_EDGE('',*,*,#15803,.T.);
#22097=ORIENTED_EDGE('',*,*,#15797,.F.);
#22098=ORIENTED_EDGE('',*,*,#15798,.F.);
#22099=ORIENTED_EDGE('',*,*,#15803,.F.);
#22100=ORIENTED_EDGE('',*,*,#15804,.T.);
#22101=ORIENTED_EDGE('',*,*,#15805,.T.);
#22102=ORIENTED_EDGE('',*,*,#15801,.F.);
#22103=ORIENTED_EDGE('',*,*,#15805,.F.);
#22104=ORIENTED_EDGE('',*,*,#15806,.F.);
#22105=ORIENTED_EDGE('',*,*,#15802,.T.);
#22106=ORIENTED_EDGE('',*,*,#15807,.F.);
#22107=ORIENTED_EDGE('',*,*,#15808,.T.);
#22108=ORIENTED_EDGE('',*,*,#15806,.T.);
#22109=ORIENTED_EDGE('',*,*,#15808,.F.);
#22110=ORIENTED_EDGE('',*,*,#15807,.T.);
#22111=ORIENTED_EDGE('',*,*,#15809,.F.);
#22112=ORIENTED_EDGE('',*,*,#15809,.T.);
#22113=ORIENTED_EDGE('',*,*,#15810,.T.);
#22114=ORIENTED_EDGE('',*,*,#15811,.F.);
#22115=ORIENTED_EDGE('',*,*,#15810,.F.);
#22116=ORIENTED_EDGE('',*,*,#15811,.T.);
#22117=ORIENTED_EDGE('',*,*,#15812,.F.);
#22118=ORIENTED_EDGE('',*,*,#15812,.T.);
#22119=ORIENTED_EDGE('',*,*,#15813,.T.);
#22120=ORIENTED_EDGE('',*,*,#15804,.F.);
#22121=ORIENTED_EDGE('',*,*,#15813,.F.);
#22122=ORIENTED_EDGE('',*,*,#15814,.T.);
#22123=ORIENTED_EDGE('',*,*,#15815,.T.);
#22124=ORIENTED_EDGE('',*,*,#15816,.T.);
#22125=ORIENTED_EDGE('',*,*,#15817,.T.);
#22126=ORIENTED_EDGE('',*,*,#15818,.T.);
#22127=ORIENTED_EDGE('',*,*,#15817,.F.);
#22128=ORIENTED_EDGE('',*,*,#15819,.T.);
#22129=ORIENTED_EDGE('',*,*,#15820,.T.);
#22130=ORIENTED_EDGE('',*,*,#15821,.T.);
#22131=ORIENTED_EDGE('',*,*,#15822,.T.);
#22132=ORIENTED_EDGE('',*,*,#15823,.T.);
#22133=ORIENTED_EDGE('',*,*,#15820,.F.);
#22134=ORIENTED_EDGE('',*,*,#15814,.F.);
#22135=ORIENTED_EDGE('',*,*,#15824,.F.);
#22136=ORIENTED_EDGE('',*,*,#15825,.F.);
#22137=ORIENTED_EDGE('',*,*,#15826,.T.);
#22138=ORIENTED_EDGE('',*,*,#15818,.F.);
#22139=ORIENTED_EDGE('',*,*,#15827,.F.);
#22140=ORIENTED_EDGE('',*,*,#15828,.F.);
#22141=ORIENTED_EDGE('',*,*,#15824,.T.);
#22142=ORIENTED_EDGE('',*,*,#15823,.F.);
#22143=ORIENTED_EDGE('',*,*,#15829,.F.);
#22144=ORIENTED_EDGE('',*,*,#15830,.F.);
#22145=ORIENTED_EDGE('',*,*,#15827,.T.);
#22146=ORIENTED_EDGE('',*,*,#15830,.T.);
#22147=ORIENTED_EDGE('',*,*,#15831,.T.);
#22148=ORIENTED_EDGE('',*,*,#15832,.T.);
#22149=ORIENTED_EDGE('',*,*,#15833,.T.);
#22150=ORIENTED_EDGE('',*,*,#15834,.T.);
#22151=ORIENTED_EDGE('',*,*,#15835,.T.);
#22152=ORIENTED_EDGE('',*,*,#15828,.T.);
#22153=ORIENTED_EDGE('',*,*,#15833,.F.);
#22154=ORIENTED_EDGE('',*,*,#15836,.T.);
#22155=ORIENTED_EDGE('',*,*,#15837,.T.);
#22156=ORIENTED_EDGE('',*,*,#15825,.T.);
#22157=ORIENTED_EDGE('',*,*,#15835,.F.);
#22158=ORIENTED_EDGE('',*,*,#15836,.F.);
#22159=ORIENTED_EDGE('',*,*,#15834,.F.);
#22160=ORIENTED_EDGE('',*,*,#15832,.F.);
#22161=ORIENTED_EDGE('',*,*,#15838,.F.);
#22162=ORIENTED_EDGE('',*,*,#15839,.F.);
#22163=ORIENTED_EDGE('',*,*,#15840,.F.);
#22164=ORIENTED_EDGE('',*,*,#15815,.F.);
#22165=ORIENTED_EDGE('',*,*,#15826,.F.);
#22166=ORIENTED_EDGE('',*,*,#15837,.F.);
#22167=ORIENTED_EDGE('',*,*,#15838,.T.);
#22168=ORIENTED_EDGE('',*,*,#15831,.F.);
#22169=ORIENTED_EDGE('',*,*,#15829,.T.);
#22170=ORIENTED_EDGE('',*,*,#15822,.F.);
#22171=ORIENTED_EDGE('',*,*,#15841,.F.);
#22172=ORIENTED_EDGE('',*,*,#15839,.T.);
#22173=ORIENTED_EDGE('',*,*,#15842,.T.);
#22174=ORIENTED_EDGE('',*,*,#15843,.T.);
#22175=ORIENTED_EDGE('',*,*,#15842,.F.);
#22176=ORIENTED_EDGE('',*,*,#15843,.F.);
#22177=ORIENTED_EDGE('',*,*,#15844,.T.);
#22178=ORIENTED_EDGE('',*,*,#15845,.F.);
#22179=ORIENTED_EDGE('',*,*,#15844,.F.);
#22180=ORIENTED_EDGE('',*,*,#15846,.T.);
#22181=ORIENTED_EDGE('',*,*,#15847,.T.);
#22182=ORIENTED_EDGE('',*,*,#15845,.T.);
#22183=ORIENTED_EDGE('',*,*,#15847,.F.);
#22184=ORIENTED_EDGE('',*,*,#15816,.F.);
#22185=ORIENTED_EDGE('',*,*,#15841,.T.);
#22186=ORIENTED_EDGE('',*,*,#15821,.F.);
#22187=ORIENTED_EDGE('',*,*,#15819,.F.);
#22188=ORIENTED_EDGE('',*,*,#15848,.F.);
#22189=ORIENTED_EDGE('',*,*,#15846,.F.);
#22190=ORIENTED_EDGE('',*,*,#15840,.T.);
#22191=ORIENTED_EDGE('',*,*,#15849,.T.);
#22192=ORIENTED_EDGE('',*,*,#15850,.T.);
#22193=ORIENTED_EDGE('',*,*,#15849,.F.);
#22194=ORIENTED_EDGE('',*,*,#15850,.F.);
#22195=ORIENTED_EDGE('',*,*,#15851,.T.);
#22196=ORIENTED_EDGE('',*,*,#15852,.F.);
#22197=ORIENTED_EDGE('',*,*,#15851,.F.);
#22198=ORIENTED_EDGE('',*,*,#15848,.T.);
#22199=ORIENTED_EDGE('',*,*,#15853,.T.);
#22200=ORIENTED_EDGE('',*,*,#15852,.T.);
#22201=ORIENTED_EDGE('',*,*,#15853,.F.);
#22202=ORIENTED_EDGE('',*,*,#15854,.T.);
#22203=ORIENTED_EDGE('',*,*,#15855,.T.);
#22204=ORIENTED_EDGE('',*,*,#15856,.T.);
#22205=ORIENTED_EDGE('',*,*,#15857,.T.);
#22206=ORIENTED_EDGE('',*,*,#15858,.T.);
#22207=ORIENTED_EDGE('',*,*,#15859,.T.);
#22208=ORIENTED_EDGE('',*,*,#15858,.F.);
#22209=ORIENTED_EDGE('',*,*,#15860,.F.);
#22210=ORIENTED_EDGE('',*,*,#15861,.F.);
#22211=ORIENTED_EDGE('',*,*,#15862,.F.);
#22212=ORIENTED_EDGE('',*,*,#15857,.F.);
#22213=ORIENTED_EDGE('',*,*,#15863,.F.);
#22214=ORIENTED_EDGE('',*,*,#15864,.T.);
#22215=ORIENTED_EDGE('',*,*,#15865,.F.);
#22216=ORIENTED_EDGE('',*,*,#15866,.F.);
#22217=ORIENTED_EDGE('',*,*,#15860,.T.);
#22218=ORIENTED_EDGE('',*,*,#15856,.F.);
#22219=ORIENTED_EDGE('',*,*,#15867,.T.);
#22220=ORIENTED_EDGE('',*,*,#15868,.F.);
#22221=ORIENTED_EDGE('',*,*,#15869,.T.);
#22222=ORIENTED_EDGE('',*,*,#15870,.T.);
#22223=ORIENTED_EDGE('',*,*,#15863,.T.);
#22224=ORIENTED_EDGE('',*,*,#15868,.T.);
#22225=ORIENTED_EDGE('',*,*,#15871,.T.);
#22226=ORIENTED_EDGE('',*,*,#15872,.T.);
#22227=ORIENTED_EDGE('',*,*,#15873,.T.);
#22228=ORIENTED_EDGE('',*,*,#15874,.T.);
#22229=ORIENTED_EDGE('',*,*,#15875,.T.);
#22230=ORIENTED_EDGE('',*,*,#15874,.F.);
#22231=ORIENTED_EDGE('',*,*,#15876,.F.);
#22232=ORIENTED_EDGE('',*,*,#15877,.F.);
#22233=ORIENTED_EDGE('',*,*,#15878,.F.);
#22234=ORIENTED_EDGE('',*,*,#15873,.F.);
#22235=ORIENTED_EDGE('',*,*,#15879,.F.);
#22236=ORIENTED_EDGE('',*,*,#15880,.T.);
#22237=ORIENTED_EDGE('',*,*,#15881,.F.);
#22238=ORIENTED_EDGE('',*,*,#15882,.F.);
#22239=ORIENTED_EDGE('',*,*,#15876,.T.);
#22240=ORIENTED_EDGE('',*,*,#15854,.F.);
#22241=ORIENTED_EDGE('',*,*,#15883,.T.);
#22242=ORIENTED_EDGE('',*,*,#15884,.T.);
#22243=ORIENTED_EDGE('',*,*,#15879,.T.);
#22244=ORIENTED_EDGE('',*,*,#15872,.F.);
#22245=ORIENTED_EDGE('',*,*,#15885,.T.);
#22246=ORIENTED_EDGE('',*,*,#15870,.F.);
#22247=ORIENTED_EDGE('',*,*,#15886,.F.);
#22248=ORIENTED_EDGE('',*,*,#15887,.F.);
#22249=ORIENTED_EDGE('',*,*,#15864,.F.);
#22250=ORIENTED_EDGE('',*,*,#15888,.T.);
#22251=ORIENTED_EDGE('',*,*,#15889,.T.);
#22252=ORIENTED_EDGE('',*,*,#15890,.T.);
#22253=ORIENTED_EDGE('',*,*,#15891,.T.);
#22254=ORIENTED_EDGE('',*,*,#15877,.T.);
#22255=ORIENTED_EDGE('',*,*,#15882,.T.);
#22256=ORIENTED_EDGE('',*,*,#15890,.F.);
#22257=ORIENTED_EDGE('',*,*,#15892,.T.);
#22258=ORIENTED_EDGE('',*,*,#15893,.T.);
#22259=ORIENTED_EDGE('',*,*,#15865,.T.);
#22260=ORIENTED_EDGE('',*,*,#15887,.T.);
#22261=ORIENTED_EDGE('',*,*,#15894,.T.);
#22262=ORIENTED_EDGE('',*,*,#15889,.F.);
#22263=ORIENTED_EDGE('',*,*,#15895,.F.);
#22264=ORIENTED_EDGE('',*,*,#15896,.F.);
#22265=ORIENTED_EDGE('',*,*,#15892,.F.);
#22266=ORIENTED_EDGE('',*,*,#15888,.F.);
#22267=ORIENTED_EDGE('',*,*,#15881,.T.);
#22268=ORIENTED_EDGE('',*,*,#15897,.T.);
#22269=ORIENTED_EDGE('',*,*,#15898,.T.);
#22270=ORIENTED_EDGE('',*,*,#15899,.F.);
#22271=ORIENTED_EDGE('',*,*,#15895,.T.);
#22272=ORIENTED_EDGE('',*,*,#15893,.F.);
#22273=ORIENTED_EDGE('',*,*,#15896,.T.);
#22274=ORIENTED_EDGE('',*,*,#15899,.T.);
#22275=ORIENTED_EDGE('',*,*,#15900,.T.);
#22276=ORIENTED_EDGE('',*,*,#15861,.T.);
#22277=ORIENTED_EDGE('',*,*,#15866,.T.);
#22278=ORIENTED_EDGE('',*,*,#15859,.F.);
#22279=ORIENTED_EDGE('',*,*,#15862,.T.);
#22280=ORIENTED_EDGE('',*,*,#15900,.F.);
#22281=ORIENTED_EDGE('',*,*,#15898,.F.);
#22282=ORIENTED_EDGE('',*,*,#15901,.T.);
#22283=ORIENTED_EDGE('',*,*,#15883,.F.);
#22284=ORIENTED_EDGE('',*,*,#15884,.F.);
#22285=ORIENTED_EDGE('',*,*,#15901,.F.);
#22286=ORIENTED_EDGE('',*,*,#15897,.F.);
#22287=ORIENTED_EDGE('',*,*,#15880,.F.);
#22288=ORIENTED_EDGE('',*,*,#15875,.F.);
#22289=ORIENTED_EDGE('',*,*,#15878,.T.);
#22290=ORIENTED_EDGE('',*,*,#15891,.F.);
#22291=ORIENTED_EDGE('',*,*,#15894,.F.);
#22292=ORIENTED_EDGE('',*,*,#15886,.T.);
#22293=ORIENTED_EDGE('',*,*,#15869,.F.);
#22294=ORIENTED_EDGE('',*,*,#15855,.F.);
#22295=ORIENTED_EDGE('',*,*,#15885,.F.);
#22296=ORIENTED_EDGE('',*,*,#15871,.F.);
#22297=ORIENTED_EDGE('',*,*,#15867,.F.);
#22298=ORIENTED_EDGE('',*,*,#15902,.F.);
#22299=ORIENTED_EDGE('',*,*,#15903,.F.);
#22300=ORIENTED_EDGE('',*,*,#15904,.T.);
#22301=ORIENTED_EDGE('',*,*,#15905,.T.);
#22302=ORIENTED_EDGE('',*,*,#15906,.T.);
#22303=ORIENTED_EDGE('',*,*,#15904,.F.);
#22304=ORIENTED_EDGE('',*,*,#15906,.F.);
#22305=ORIENTED_EDGE('',*,*,#15907,.T.);
#22306=ORIENTED_EDGE('',*,*,#15908,.T.);
#22307=ORIENTED_EDGE('',*,*,#15909,.T.);
#22308=ORIENTED_EDGE('',*,*,#15907,.F.);
#22309=ORIENTED_EDGE('',*,*,#15905,.F.);
#22310=ORIENTED_EDGE('',*,*,#15908,.F.);
#22311=ORIENTED_EDGE('',*,*,#15909,.F.);
#22312=ORIENTED_EDGE('',*,*,#15910,.T.);
#22313=ORIENTED_EDGE('',*,*,#15911,.T.);
#22314=ORIENTED_EDGE('',*,*,#15912,.T.);
#22315=ORIENTED_EDGE('',*,*,#15910,.F.);
#22316=ORIENTED_EDGE('',*,*,#15912,.F.);
#22317=ORIENTED_EDGE('',*,*,#15913,.T.);
#22318=ORIENTED_EDGE('',*,*,#15902,.T.);
#22319=ORIENTED_EDGE('',*,*,#15903,.T.);
#22320=ORIENTED_EDGE('',*,*,#15913,.F.);
#22321=ORIENTED_EDGE('',*,*,#15911,.F.);
#22322=ORIENTED_EDGE('',*,*,#15914,.F.);
#22323=ORIENTED_EDGE('',*,*,#15915,.F.);
#22324=ORIENTED_EDGE('',*,*,#15916,.F.);
#22325=ORIENTED_EDGE('',*,*,#15917,.F.);
#22326=ORIENTED_EDGE('',*,*,#15918,.F.);
#22327=ORIENTED_EDGE('',*,*,#15919,.F.);
#22328=ORIENTED_EDGE('',*,*,#15920,.F.);
#22329=ORIENTED_EDGE('',*,*,#15921,.F.);
#22330=ORIENTED_EDGE('',*,*,#15922,.F.);
#22331=ORIENTED_EDGE('',*,*,#15923,.F.);
#22332=ORIENTED_EDGE('',*,*,#15924,.F.);
#22333=ORIENTED_EDGE('',*,*,#15925,.F.);
#22334=ORIENTED_EDGE('',*,*,#15924,.T.);
#22335=ORIENTED_EDGE('',*,*,#15926,.T.);
#22336=ORIENTED_EDGE('',*,*,#15918,.T.);
#22337=ORIENTED_EDGE('',*,*,#15927,.T.);
#22338=ORIENTED_EDGE('',*,*,#15928,.F.);
#22339=ORIENTED_EDGE('',*,*,#15929,.F.);
#22340=ORIENTED_EDGE('',*,*,#15930,.F.);
#22341=ORIENTED_EDGE('',*,*,#15931,.F.);
#22342=ORIENTED_EDGE('',*,*,#15932,.F.);
#22343=ORIENTED_EDGE('',*,*,#15933,.F.);
#22344=ORIENTED_EDGE('',*,*,#15932,.T.);
#22345=ORIENTED_EDGE('',*,*,#15934,.T.);
#22346=ORIENTED_EDGE('',*,*,#15925,.T.);
#22347=ORIENTED_EDGE('',*,*,#15935,.T.);
#22348=ORIENTED_EDGE('',*,*,#15929,.T.);
#22349=ORIENTED_EDGE('',*,*,#15936,.T.);
#22350=ORIENTED_EDGE('',*,*,#15933,.T.);
#22351=ORIENTED_EDGE('',*,*,#15937,.T.);
#22352=ORIENTED_EDGE('',*,*,#15938,.T.);
#22353=ORIENTED_EDGE('',*,*,#15939,.T.);
#22354=ORIENTED_EDGE('',*,*,#15931,.T.);
#22355=ORIENTED_EDGE('',*,*,#15940,.T.);
#22356=ORIENTED_EDGE('',*,*,#15921,.T.);
#22357=ORIENTED_EDGE('',*,*,#15941,.T.);
#22358=ORIENTED_EDGE('',*,*,#15930,.T.);
#22359=ORIENTED_EDGE('',*,*,#15942,.T.);
#22360=ORIENTED_EDGE('',*,*,#15943,.T.);
#22361=ORIENTED_EDGE('',*,*,#15944,.T.);
#22362=ORIENTED_EDGE('',*,*,#15928,.T.);
#22363=ORIENTED_EDGE('',*,*,#15945,.T.);
#22364=ORIENTED_EDGE('',*,*,#15946,.T.);
#22365=ORIENTED_EDGE('',*,*,#15947,.T.);
#22366=ORIENTED_EDGE('',*,*,#15923,.T.);
#22367=ORIENTED_EDGE('',*,*,#15948,.T.);
#22368=ORIENTED_EDGE('',*,*,#15915,.T.);
#22369=ORIENTED_EDGE('',*,*,#15949,.T.);
#22370=ORIENTED_EDGE('',*,*,#15922,.T.);
#22371=ORIENTED_EDGE('',*,*,#15950,.T.);
#22372=ORIENTED_EDGE('',*,*,#15951,.T.);
#22373=ORIENTED_EDGE('',*,*,#15952,.T.);
#22374=ORIENTED_EDGE('',*,*,#15920,.T.);
#22375=ORIENTED_EDGE('',*,*,#15953,.T.);
#22376=ORIENTED_EDGE('',*,*,#15954,.T.);
#22377=ORIENTED_EDGE('',*,*,#15955,.T.);
#22378=ORIENTED_EDGE('',*,*,#15919,.T.);
#22379=ORIENTED_EDGE('',*,*,#15956,.T.);
#22380=ORIENTED_EDGE('',*,*,#15917,.T.);
#22381=ORIENTED_EDGE('',*,*,#15957,.T.);
#22382=ORIENTED_EDGE('',*,*,#15916,.T.);
#22383=ORIENTED_EDGE('',*,*,#15958,.T.);
#22384=ORIENTED_EDGE('',*,*,#15959,.T.);
#22385=ORIENTED_EDGE('',*,*,#15960,.T.);
#22386=ORIENTED_EDGE('',*,*,#15914,.T.);
#22387=ORIENTED_EDGE('',*,*,#15961,.T.);
#22388=ORIENTED_EDGE('',*,*,#15940,.F.);
#22389=ORIENTED_EDGE('',*,*,#15936,.F.);
#22390=ORIENTED_EDGE('',*,*,#15944,.F.);
#22391=ORIENTED_EDGE('',*,*,#15962,.T.);
#22392=ORIENTED_EDGE('',*,*,#15945,.F.);
#22393=ORIENTED_EDGE('',*,*,#15941,.F.);
#22394=ORIENTED_EDGE('',*,*,#15952,.F.);
#22395=ORIENTED_EDGE('',*,*,#15963,.T.);
#22396=ORIENTED_EDGE('',*,*,#15964,.T.);
#22397=ORIENTED_EDGE('',*,*,#15953,.F.);
#22398=ORIENTED_EDGE('',*,*,#15949,.F.);
#22399=ORIENTED_EDGE('',*,*,#15960,.F.);
#22400=ORIENTED_EDGE('',*,*,#15965,.T.);
#22401=ORIENTED_EDGE('',*,*,#15927,.F.);
#22402=ORIENTED_EDGE('',*,*,#15958,.F.);
#22403=ORIENTED_EDGE('',*,*,#15950,.F.);
#22404=ORIENTED_EDGE('',*,*,#15942,.F.);
#22405=ORIENTED_EDGE('',*,*,#15937,.F.);
#22406=ORIENTED_EDGE('',*,*,#15935,.F.);
#22407=ORIENTED_EDGE('',*,*,#15966,.T.);
#22408=ORIENTED_EDGE('',*,*,#15967,.T.);
#22409=ORIENTED_EDGE('',*,*,#15968,.T.);
#22410=ORIENTED_EDGE('',*,*,#15969,.T.);
#22411=ORIENTED_EDGE('',*,*,#15970,.F.);
#22412=ORIENTED_EDGE('',*,*,#15971,.T.);
#22413=ORIENTED_EDGE('',*,*,#15972,.T.);
#22414=ORIENTED_EDGE('',*,*,#15973,.T.);
#22415=ORIENTED_EDGE('',*,*,#15968,.F.);
#22416=ORIENTED_EDGE('',*,*,#15974,.T.);
#22417=ORIENTED_EDGE('',*,*,#15975,.T.);
#22418=ORIENTED_EDGE('',*,*,#15976,.T.);
#22419=ORIENTED_EDGE('',*,*,#15977,.T.);
#22420=ORIENTED_EDGE('',*,*,#15978,.T.);
#22421=ORIENTED_EDGE('',*,*,#15975,.F.);
#22422=ORIENTED_EDGE('',*,*,#15979,.T.);
#22423=ORIENTED_EDGE('',*,*,#15980,.T.);
#22424=ORIENTED_EDGE('',*,*,#15981,.T.);
#22425=ORIENTED_EDGE('',*,*,#15977,.F.);
#22426=ORIENTED_EDGE('',*,*,#15982,.T.);
#22427=ORIENTED_EDGE('',*,*,#15972,.F.);
#22428=ORIENTED_EDGE('',*,*,#15983,.T.);
#22429=ORIENTED_EDGE('',*,*,#15980,.F.);
#22430=ORIENTED_EDGE('',*,*,#15984,.T.);
#22431=ORIENTED_EDGE('',*,*,#15970,.T.);
#22432=ORIENTED_EDGE('',*,*,#15973,.F.);
#22433=ORIENTED_EDGE('',*,*,#15985,.T.);
#22434=ORIENTED_EDGE('',*,*,#15986,.T.);
#22435=ORIENTED_EDGE('',*,*,#15987,.F.);
#22436=ORIENTED_EDGE('',*,*,#15982,.F.);
#22437=ORIENTED_EDGE('',*,*,#15988,.T.);
#22438=ORIENTED_EDGE('',*,*,#15989,.T.);
#22439=ORIENTED_EDGE('',*,*,#15985,.F.);
#22440=ORIENTED_EDGE('',*,*,#15976,.F.);
#22441=ORIENTED_EDGE('',*,*,#15990,.T.);
#22442=ORIENTED_EDGE('',*,*,#15991,.T.);
#22443=ORIENTED_EDGE('',*,*,#15988,.F.);
#22444=ORIENTED_EDGE('',*,*,#15992,.T.);
#22445=ORIENTED_EDGE('',*,*,#15974,.F.);
#22446=ORIENTED_EDGE('',*,*,#15981,.F.);
#22447=ORIENTED_EDGE('',*,*,#15971,.F.);
#22448=ORIENTED_EDGE('',*,*,#15967,.F.);
#22449=ORIENTED_EDGE('',*,*,#15984,.F.);
#22450=ORIENTED_EDGE('',*,*,#15979,.F.);
#22451=ORIENTED_EDGE('',*,*,#15978,.F.);
#22452=ORIENTED_EDGE('',*,*,#15993,.T.);
#22453=ORIENTED_EDGE('',*,*,#15994,.T.);
#22454=ORIENTED_EDGE('',*,*,#15990,.F.);
#22455=ORIENTED_EDGE('',*,*,#15983,.F.);
#22456=ORIENTED_EDGE('',*,*,#15995,.T.);
#22457=ORIENTED_EDGE('',*,*,#15996,.T.);
#22458=ORIENTED_EDGE('',*,*,#15993,.F.);
#22459=ORIENTED_EDGE('',*,*,#15969,.F.);
#22460=ORIENTED_EDGE('',*,*,#15987,.T.);
#22461=ORIENTED_EDGE('',*,*,#15997,.T.);
#22462=ORIENTED_EDGE('',*,*,#15995,.F.);
#22463=ORIENTED_EDGE('',*,*,#15989,.F.);
#22464=ORIENTED_EDGE('',*,*,#15991,.F.);
#22465=ORIENTED_EDGE('',*,*,#15994,.F.);
#22466=ORIENTED_EDGE('',*,*,#15996,.F.);
#22467=ORIENTED_EDGE('',*,*,#15997,.F.);
#22468=ORIENTED_EDGE('',*,*,#15986,.F.);
#22469=ORIENTED_EDGE('',*,*,#15938,.F.);
#22470=ORIENTED_EDGE('',*,*,#15962,.F.);
#22471=ORIENTED_EDGE('',*,*,#15943,.F.);
#22472=ORIENTED_EDGE('',*,*,#15964,.F.);
#22473=ORIENTED_EDGE('',*,*,#15998,.T.);
#22474=ORIENTED_EDGE('',*,*,#15992,.F.);
#22475=ORIENTED_EDGE('',*,*,#15998,.F.);
#22476=ORIENTED_EDGE('',*,*,#15963,.F.);
#22477=ORIENTED_EDGE('',*,*,#15951,.F.);
#22478=ORIENTED_EDGE('',*,*,#15965,.F.);
#22479=ORIENTED_EDGE('',*,*,#15959,.F.);
#22480=ORIENTED_EDGE('',*,*,#15999,.F.);
#22481=ORIENTED_EDGE('',*,*,#15954,.F.);
#22482=ORIENTED_EDGE('',*,*,#16000,.F.);
#22483=ORIENTED_EDGE('',*,*,#15946,.F.);
#22484=ORIENTED_EDGE('',*,*,#16001,.F.);
#22485=ORIENTED_EDGE('',*,*,#15939,.F.);
#22486=ORIENTED_EDGE('',*,*,#16001,.T.);
#22487=ORIENTED_EDGE('',*,*,#15948,.F.);
#22488=ORIENTED_EDGE('',*,*,#15934,.F.);
#22489=ORIENTED_EDGE('',*,*,#15947,.F.);
#22490=ORIENTED_EDGE('',*,*,#16000,.T.);
#22491=ORIENTED_EDGE('',*,*,#15956,.F.);
#22492=ORIENTED_EDGE('',*,*,#15926,.F.);
#22493=ORIENTED_EDGE('',*,*,#15955,.F.);
#22494=ORIENTED_EDGE('',*,*,#15999,.T.);
#22495=ORIENTED_EDGE('',*,*,#15961,.F.);
#22496=ORIENTED_EDGE('',*,*,#15957,.F.);
#22497=ORIENTED_EDGE('',*,*,#16002,.F.);
#22498=ORIENTED_EDGE('',*,*,#16003,.F.);
#22499=ORIENTED_EDGE('',*,*,#16004,.T.);
#22500=ORIENTED_EDGE('',*,*,#16002,.T.);
#22501=ORIENTED_EDGE('',*,*,#16004,.F.);
#22502=ORIENTED_EDGE('',*,*,#16005,.F.);
#22503=ORIENTED_EDGE('',*,*,#16006,.T.);
#22504=ORIENTED_EDGE('',*,*,#16003,.T.);
#22505=ORIENTED_EDGE('',*,*,#16006,.F.);
#22506=ORIENTED_EDGE('',*,*,#16005,.T.);
#22507=ORIENTED_EDGE('',*,*,#16007,.F.);
#22508=ORIENTED_EDGE('',*,*,#15966,.F.);
#22509=ORIENTED_EDGE('',*,*,#16008,.T.);
#22510=ORIENTED_EDGE('',*,*,#16007,.T.);
#22511=ORIENTED_EDGE('',*,*,#16008,.F.);
#22512=ORIENTED_EDGE('',*,*,#16009,.T.);
#22513=ORIENTED_EDGE('',*,*,#16010,.T.);
#22514=ORIENTED_EDGE('',*,*,#16011,.F.);
#22515=ORIENTED_EDGE('',*,*,#16010,.F.);
#22516=ORIENTED_EDGE('',*,*,#16012,.F.);
#22517=ORIENTED_EDGE('',*,*,#16011,.T.);
#22518=ORIENTED_EDGE('',*,*,#16013,.F.);
#22519=ORIENTED_EDGE('',*,*,#16009,.F.);
#22520=ORIENTED_EDGE('',*,*,#16014,.T.);
#22521=ORIENTED_EDGE('',*,*,#16015,.T.);
#22522=ORIENTED_EDGE('',*,*,#16013,.T.);
#22523=ORIENTED_EDGE('',*,*,#16015,.F.);
#22524=ORIENTED_EDGE('',*,*,#16016,.T.);
#22525=ORIENTED_EDGE('',*,*,#16017,.T.);
#22526=ORIENTED_EDGE('',*,*,#16018,.F.);
#22527=ORIENTED_EDGE('',*,*,#16017,.F.);
#22528=ORIENTED_EDGE('',*,*,#16019,.F.);
#22529=ORIENTED_EDGE('',*,*,#16018,.T.);
#22530=ORIENTED_EDGE('',*,*,#16020,.F.);
#22531=ORIENTED_EDGE('',*,*,#16021,.T.);
#22532=ORIENTED_EDGE('',*,*,#16019,.T.);
#22533=ORIENTED_EDGE('',*,*,#16021,.F.);
#22534=ORIENTED_EDGE('',*,*,#16020,.T.);
#22535=ORIENTED_EDGE('',*,*,#16022,.F.);
#22536=ORIENTED_EDGE('',*,*,#16022,.T.);
#22537=ORIENTED_EDGE('',*,*,#16023,.T.);
#22538=ORIENTED_EDGE('',*,*,#16024,.F.);
#22539=ORIENTED_EDGE('',*,*,#16023,.F.);
#22540=ORIENTED_EDGE('',*,*,#16014,.F.);
#22541=ORIENTED_EDGE('',*,*,#16024,.T.);
#22542=ORIENTED_EDGE('',*,*,#16012,.T.);
#22543=ORIENTED_EDGE('',*,*,#16025,.T.);
#22544=ORIENTED_EDGE('',*,*,#16026,.F.);
#22545=ORIENTED_EDGE('',*,*,#16025,.F.);
#22546=ORIENTED_EDGE('',*,*,#16026,.T.);
#22547=ORIENTED_EDGE('',*,*,#16016,.F.);
#22548=ORIENTED_EDGE('',*,*,#16027,.F.);
#22549=ORIENTED_EDGE('',*,*,#16028,.T.);
#22550=ORIENTED_EDGE('',*,*,#16029,.T.);
#22551=ORIENTED_EDGE('',*,*,#16030,.T.);
#22552=ORIENTED_EDGE('',*,*,#16031,.F.);
#22553=ORIENTED_EDGE('',*,*,#16032,.T.);
#22554=ORIENTED_EDGE('',*,*,#16027,.T.);
#22555=ORIENTED_EDGE('',*,*,#16033,.T.);
#22556=ORIENTED_EDGE('',*,*,#16034,.F.);
#22557=ORIENTED_EDGE('',*,*,#16035,.T.);
#22558=ORIENTED_EDGE('',*,*,#16031,.T.);
#22559=ORIENTED_EDGE('',*,*,#16036,.T.);
#22560=ORIENTED_EDGE('',*,*,#16037,.F.);
#22561=ORIENTED_EDGE('',*,*,#16038,.T.);
#22562=ORIENTED_EDGE('',*,*,#16034,.T.);
#22563=ORIENTED_EDGE('',*,*,#16039,.T.);
#22564=ORIENTED_EDGE('',*,*,#16040,.F.);
#22565=ORIENTED_EDGE('',*,*,#16041,.T.);
#22566=ORIENTED_EDGE('',*,*,#16037,.T.);
#22567=ORIENTED_EDGE('',*,*,#16042,.T.);
#22568=ORIENTED_EDGE('',*,*,#16043,.F.);
#22569=ORIENTED_EDGE('',*,*,#16044,.T.);
#22570=ORIENTED_EDGE('',*,*,#16040,.T.);
#22571=ORIENTED_EDGE('',*,*,#16045,.T.);
#22572=ORIENTED_EDGE('',*,*,#16046,.F.);
#22573=ORIENTED_EDGE('',*,*,#16047,.T.);
#22574=ORIENTED_EDGE('',*,*,#16043,.T.);
#22575=ORIENTED_EDGE('',*,*,#16048,.T.);
#22576=ORIENTED_EDGE('',*,*,#16049,.F.);
#22577=ORIENTED_EDGE('',*,*,#16050,.T.);
#22578=ORIENTED_EDGE('',*,*,#16046,.T.);
#22579=ORIENTED_EDGE('',*,*,#16051,.T.);
#22580=ORIENTED_EDGE('',*,*,#16052,.F.);
#22581=ORIENTED_EDGE('',*,*,#16053,.T.);
#22582=ORIENTED_EDGE('',*,*,#16049,.T.);
#22583=ORIENTED_EDGE('',*,*,#16054,.T.);
#22584=ORIENTED_EDGE('',*,*,#16055,.F.);
#22585=ORIENTED_EDGE('',*,*,#16056,.T.);
#22586=ORIENTED_EDGE('',*,*,#16052,.T.);
#22587=ORIENTED_EDGE('',*,*,#16057,.T.);
#22588=ORIENTED_EDGE('',*,*,#16058,.F.);
#22589=ORIENTED_EDGE('',*,*,#16059,.T.);
#22590=ORIENTED_EDGE('',*,*,#16055,.T.);
#22591=ORIENTED_EDGE('',*,*,#16060,.T.);
#22592=ORIENTED_EDGE('',*,*,#16061,.F.);
#22593=ORIENTED_EDGE('',*,*,#16062,.T.);
#22594=ORIENTED_EDGE('',*,*,#16058,.T.);
#22595=ORIENTED_EDGE('',*,*,#16063,.T.);
#22596=ORIENTED_EDGE('',*,*,#16064,.F.);
#22597=ORIENTED_EDGE('',*,*,#16065,.T.);
#22598=ORIENTED_EDGE('',*,*,#16061,.T.);
#22599=ORIENTED_EDGE('',*,*,#16066,.T.);
#22600=ORIENTED_EDGE('',*,*,#16067,.F.);
#22601=ORIENTED_EDGE('',*,*,#16068,.T.);
#22602=ORIENTED_EDGE('',*,*,#16064,.T.);
#22603=ORIENTED_EDGE('',*,*,#16069,.T.);
#22604=ORIENTED_EDGE('',*,*,#16070,.F.);
#22605=ORIENTED_EDGE('',*,*,#16071,.T.);
#22606=ORIENTED_EDGE('',*,*,#16067,.T.);
#22607=ORIENTED_EDGE('',*,*,#16072,.T.);
#22608=ORIENTED_EDGE('',*,*,#16073,.F.);
#22609=ORIENTED_EDGE('',*,*,#16074,.T.);
#22610=ORIENTED_EDGE('',*,*,#16070,.T.);
#22611=ORIENTED_EDGE('',*,*,#16075,.T.);
#22612=ORIENTED_EDGE('',*,*,#16076,.F.);
#22613=ORIENTED_EDGE('',*,*,#16077,.T.);
#22614=ORIENTED_EDGE('',*,*,#16073,.T.);
#22615=ORIENTED_EDGE('',*,*,#16078,.T.);
#22616=ORIENTED_EDGE('',*,*,#16079,.F.);
#22617=ORIENTED_EDGE('',*,*,#16080,.T.);
#22618=ORIENTED_EDGE('',*,*,#16076,.T.);
#22619=ORIENTED_EDGE('',*,*,#16081,.T.);
#22620=ORIENTED_EDGE('',*,*,#16082,.F.);
#22621=ORIENTED_EDGE('',*,*,#16083,.T.);
#22622=ORIENTED_EDGE('',*,*,#16079,.T.);
#22623=ORIENTED_EDGE('',*,*,#16084,.T.);
#22624=ORIENTED_EDGE('',*,*,#16085,.F.);
#22625=ORIENTED_EDGE('',*,*,#16086,.T.);
#22626=ORIENTED_EDGE('',*,*,#16082,.T.);
#22627=ORIENTED_EDGE('',*,*,#16087,.T.);
#22628=ORIENTED_EDGE('',*,*,#16088,.F.);
#22629=ORIENTED_EDGE('',*,*,#16089,.F.);
#22630=ORIENTED_EDGE('',*,*,#16090,.T.);
#22631=ORIENTED_EDGE('',*,*,#16085,.T.);
#22632=ORIENTED_EDGE('',*,*,#16091,.T.);
#22633=ORIENTED_EDGE('',*,*,#16092,.F.);
#22634=ORIENTED_EDGE('',*,*,#16093,.T.);
#22635=ORIENTED_EDGE('',*,*,#16094,.F.);
#22636=ORIENTED_EDGE('',*,*,#16095,.F.);
#22637=ORIENTED_EDGE('',*,*,#16096,.F.);
#22638=ORIENTED_EDGE('',*,*,#16097,.T.);
#22639=ORIENTED_EDGE('',*,*,#16092,.T.);
#22640=ORIENTED_EDGE('',*,*,#16098,.F.);
#22641=ORIENTED_EDGE('',*,*,#16099,.F.);
#22642=ORIENTED_EDGE('',*,*,#16100,.T.);
#22643=ORIENTED_EDGE('',*,*,#16096,.T.);
#22644=ORIENTED_EDGE('',*,*,#16101,.F.);
#22645=ORIENTED_EDGE('',*,*,#16102,.F.);
#22646=ORIENTED_EDGE('',*,*,#16103,.T.);
#22647=ORIENTED_EDGE('',*,*,#16099,.T.);
#22648=ORIENTED_EDGE('',*,*,#16104,.F.);
#22649=ORIENTED_EDGE('',*,*,#16105,.F.);
#22650=ORIENTED_EDGE('',*,*,#16106,.T.);
#22651=ORIENTED_EDGE('',*,*,#16102,.T.);
#22652=ORIENTED_EDGE('',*,*,#16107,.F.);
#22653=ORIENTED_EDGE('',*,*,#16108,.F.);
#22654=ORIENTED_EDGE('',*,*,#16109,.T.);
#22655=ORIENTED_EDGE('',*,*,#16105,.T.);
#22656=ORIENTED_EDGE('',*,*,#16110,.F.);
#22657=ORIENTED_EDGE('',*,*,#16111,.F.);
#22658=ORIENTED_EDGE('',*,*,#16112,.T.);
#22659=ORIENTED_EDGE('',*,*,#16108,.T.);
#22660=ORIENTED_EDGE('',*,*,#16113,.F.);
#22661=ORIENTED_EDGE('',*,*,#16114,.F.);
#22662=ORIENTED_EDGE('',*,*,#16115,.T.);
#22663=ORIENTED_EDGE('',*,*,#16111,.T.);
#22664=ORIENTED_EDGE('',*,*,#16116,.F.);
#22665=ORIENTED_EDGE('',*,*,#16117,.F.);
#22666=ORIENTED_EDGE('',*,*,#16118,.T.);
#22667=ORIENTED_EDGE('',*,*,#16114,.T.);
#22668=ORIENTED_EDGE('',*,*,#16119,.F.);
#22669=ORIENTED_EDGE('',*,*,#16120,.F.);
#22670=ORIENTED_EDGE('',*,*,#16121,.T.);
#22671=ORIENTED_EDGE('',*,*,#16117,.T.);
#22672=ORIENTED_EDGE('',*,*,#16122,.F.);
#22673=ORIENTED_EDGE('',*,*,#16123,.F.);
#22674=ORIENTED_EDGE('',*,*,#16124,.T.);
#22675=ORIENTED_EDGE('',*,*,#16120,.T.);
#22676=ORIENTED_EDGE('',*,*,#16125,.F.);
#22677=ORIENTED_EDGE('',*,*,#16126,.F.);
#22678=ORIENTED_EDGE('',*,*,#16127,.T.);
#22679=ORIENTED_EDGE('',*,*,#16123,.T.);
#22680=ORIENTED_EDGE('',*,*,#16128,.F.);
#22681=ORIENTED_EDGE('',*,*,#16129,.F.);
#22682=ORIENTED_EDGE('',*,*,#16130,.T.);
#22683=ORIENTED_EDGE('',*,*,#16126,.T.);
#22684=ORIENTED_EDGE('',*,*,#16131,.F.);
#22685=ORIENTED_EDGE('',*,*,#16132,.F.);
#22686=ORIENTED_EDGE('',*,*,#16133,.T.);
#22687=ORIENTED_EDGE('',*,*,#16129,.T.);
#22688=ORIENTED_EDGE('',*,*,#16134,.F.);
#22689=ORIENTED_EDGE('',*,*,#16135,.F.);
#22690=ORIENTED_EDGE('',*,*,#16136,.T.);
#22691=ORIENTED_EDGE('',*,*,#16132,.T.);
#22692=ORIENTED_EDGE('',*,*,#16137,.F.);
#22693=ORIENTED_EDGE('',*,*,#16138,.F.);
#22694=ORIENTED_EDGE('',*,*,#16139,.T.);
#22695=ORIENTED_EDGE('',*,*,#16135,.T.);
#22696=ORIENTED_EDGE('',*,*,#16140,.F.);
#22697=ORIENTED_EDGE('',*,*,#16141,.F.);
#22698=ORIENTED_EDGE('',*,*,#16142,.T.);
#22699=ORIENTED_EDGE('',*,*,#16138,.T.);
#22700=ORIENTED_EDGE('',*,*,#16143,.F.);
#22701=ORIENTED_EDGE('',*,*,#16144,.F.);
#22702=ORIENTED_EDGE('',*,*,#16145,.T.);
#22703=ORIENTED_EDGE('',*,*,#16141,.T.);
#22704=ORIENTED_EDGE('',*,*,#16146,.F.);
#22705=ORIENTED_EDGE('',*,*,#16147,.F.);
#22706=ORIENTED_EDGE('',*,*,#16148,.T.);
#22707=ORIENTED_EDGE('',*,*,#16144,.T.);
#22708=ORIENTED_EDGE('',*,*,#16149,.F.);
#22709=ORIENTED_EDGE('',*,*,#16150,.F.);
#22710=ORIENTED_EDGE('',*,*,#16151,.T.);
#22711=ORIENTED_EDGE('',*,*,#16147,.T.);
#22712=ORIENTED_EDGE('',*,*,#16152,.F.);
#22713=ORIENTED_EDGE('',*,*,#16094,.T.);
#22714=ORIENTED_EDGE('',*,*,#16153,.T.);
#22715=ORIENTED_EDGE('',*,*,#16154,.F.);
#22716=ORIENTED_EDGE('',*,*,#16155,.T.);
#22717=ORIENTED_EDGE('',*,*,#16155,.F.);
#22718=ORIENTED_EDGE('',*,*,#16156,.F.);
#22719=ORIENTED_EDGE('',*,*,#16091,.F.);
#22720=ORIENTED_EDGE('',*,*,#16087,.F.);
#22721=ORIENTED_EDGE('',*,*,#16084,.F.);
#22722=ORIENTED_EDGE('',*,*,#16081,.F.);
#22723=ORIENTED_EDGE('',*,*,#16078,.F.);
#22724=ORIENTED_EDGE('',*,*,#16075,.F.);
#22725=ORIENTED_EDGE('',*,*,#16072,.F.);
#22726=ORIENTED_EDGE('',*,*,#16069,.F.);
#22727=ORIENTED_EDGE('',*,*,#16066,.F.);
#22728=ORIENTED_EDGE('',*,*,#16063,.F.);
#22729=ORIENTED_EDGE('',*,*,#16060,.F.);
#22730=ORIENTED_EDGE('',*,*,#16057,.F.);
#22731=ORIENTED_EDGE('',*,*,#16054,.F.);
#22732=ORIENTED_EDGE('',*,*,#16051,.F.);
#22733=ORIENTED_EDGE('',*,*,#16048,.F.);
#22734=ORIENTED_EDGE('',*,*,#16045,.F.);
#22735=ORIENTED_EDGE('',*,*,#16042,.F.);
#22736=ORIENTED_EDGE('',*,*,#16039,.F.);
#22737=ORIENTED_EDGE('',*,*,#16036,.F.);
#22738=ORIENTED_EDGE('',*,*,#16033,.F.);
#22739=ORIENTED_EDGE('',*,*,#16030,.F.);
#22740=ORIENTED_EDGE('',*,*,#16157,.F.);
#22741=ORIENTED_EDGE('',*,*,#16158,.T.);
#22742=ORIENTED_EDGE('',*,*,#16152,.T.);
#22743=ORIENTED_EDGE('',*,*,#16149,.T.);
#22744=ORIENTED_EDGE('',*,*,#16146,.T.);
#22745=ORIENTED_EDGE('',*,*,#16143,.T.);
#22746=ORIENTED_EDGE('',*,*,#16140,.T.);
#22747=ORIENTED_EDGE('',*,*,#16137,.T.);
#22748=ORIENTED_EDGE('',*,*,#16134,.T.);
#22749=ORIENTED_EDGE('',*,*,#16131,.T.);
#22750=ORIENTED_EDGE('',*,*,#16128,.T.);
#22751=ORIENTED_EDGE('',*,*,#16125,.T.);
#22752=ORIENTED_EDGE('',*,*,#16122,.T.);
#22753=ORIENTED_EDGE('',*,*,#16119,.T.);
#22754=ORIENTED_EDGE('',*,*,#16116,.T.);
#22755=ORIENTED_EDGE('',*,*,#16113,.T.);
#22756=ORIENTED_EDGE('',*,*,#16110,.T.);
#22757=ORIENTED_EDGE('',*,*,#16107,.T.);
#22758=ORIENTED_EDGE('',*,*,#16104,.T.);
#22759=ORIENTED_EDGE('',*,*,#16101,.T.);
#22760=ORIENTED_EDGE('',*,*,#16098,.T.);
#22761=ORIENTED_EDGE('',*,*,#16095,.T.);
#22762=ORIENTED_EDGE('',*,*,#16159,.T.);
#22763=ORIENTED_EDGE('',*,*,#16160,.T.);
#22764=ORIENTED_EDGE('',*,*,#16161,.T.);
#22765=ORIENTED_EDGE('',*,*,#16162,.T.);
#22766=ORIENTED_EDGE('',*,*,#16157,.T.);
#22767=ORIENTED_EDGE('',*,*,#16150,.T.);
#22768=ORIENTED_EDGE('',*,*,#16158,.F.);
#22769=ORIENTED_EDGE('',*,*,#16162,.F.);
#22770=ORIENTED_EDGE('',*,*,#16163,.T.);
#22771=ORIENTED_EDGE('',*,*,#16153,.F.);
#22772=ORIENTED_EDGE('',*,*,#16093,.F.);
#22773=ORIENTED_EDGE('',*,*,#16097,.F.);
#22774=ORIENTED_EDGE('',*,*,#16100,.F.);
#22775=ORIENTED_EDGE('',*,*,#16103,.F.);
#22776=ORIENTED_EDGE('',*,*,#16106,.F.);
#22777=ORIENTED_EDGE('',*,*,#16109,.F.);
#22778=ORIENTED_EDGE('',*,*,#16112,.F.);
#22779=ORIENTED_EDGE('',*,*,#16115,.F.);
#22780=ORIENTED_EDGE('',*,*,#16118,.F.);
#22781=ORIENTED_EDGE('',*,*,#16121,.F.);
#22782=ORIENTED_EDGE('',*,*,#16124,.F.);
#22783=ORIENTED_EDGE('',*,*,#16127,.F.);
#22784=ORIENTED_EDGE('',*,*,#16130,.F.);
#22785=ORIENTED_EDGE('',*,*,#16133,.F.);
#22786=ORIENTED_EDGE('',*,*,#16136,.F.);
#22787=ORIENTED_EDGE('',*,*,#16139,.F.);
#22788=ORIENTED_EDGE('',*,*,#16142,.F.);
#22789=ORIENTED_EDGE('',*,*,#16145,.F.);
#22790=ORIENTED_EDGE('',*,*,#16148,.F.);
#22791=ORIENTED_EDGE('',*,*,#16151,.F.);
#22792=ORIENTED_EDGE('',*,*,#16163,.F.);
#22793=ORIENTED_EDGE('',*,*,#16161,.F.);
#22794=ORIENTED_EDGE('',*,*,#16028,.F.);
#22795=ORIENTED_EDGE('',*,*,#16032,.F.);
#22796=ORIENTED_EDGE('',*,*,#16035,.F.);
#22797=ORIENTED_EDGE('',*,*,#16038,.F.);
#22798=ORIENTED_EDGE('',*,*,#16041,.F.);
#22799=ORIENTED_EDGE('',*,*,#16044,.F.);
#22800=ORIENTED_EDGE('',*,*,#16047,.F.);
#22801=ORIENTED_EDGE('',*,*,#16050,.F.);
#22802=ORIENTED_EDGE('',*,*,#16053,.F.);
#22803=ORIENTED_EDGE('',*,*,#16056,.F.);
#22804=ORIENTED_EDGE('',*,*,#16059,.F.);
#22805=ORIENTED_EDGE('',*,*,#16062,.F.);
#22806=ORIENTED_EDGE('',*,*,#16065,.F.);
#22807=ORIENTED_EDGE('',*,*,#16068,.F.);
#22808=ORIENTED_EDGE('',*,*,#16071,.F.);
#22809=ORIENTED_EDGE('',*,*,#16074,.F.);
#22810=ORIENTED_EDGE('',*,*,#16077,.F.);
#22811=ORIENTED_EDGE('',*,*,#16080,.F.);
#22812=ORIENTED_EDGE('',*,*,#16083,.F.);
#22813=ORIENTED_EDGE('',*,*,#16086,.F.);
#22814=ORIENTED_EDGE('',*,*,#16090,.F.);
#22815=ORIENTED_EDGE('',*,*,#16164,.F.);
#22816=ORIENTED_EDGE('',*,*,#16165,.T.);
#22817=ORIENTED_EDGE('',*,*,#16166,.F.);
#22818=ORIENTED_EDGE('',*,*,#16167,.F.);
#22819=ORIENTED_EDGE('',*,*,#16168,.F.);
#22820=ORIENTED_EDGE('',*,*,#16167,.T.);
#22821=ORIENTED_EDGE('',*,*,#16169,.T.);
#22822=ORIENTED_EDGE('',*,*,#16170,.F.);
#22823=ORIENTED_EDGE('',*,*,#16169,.F.);
#22824=ORIENTED_EDGE('',*,*,#16166,.T.);
#22825=ORIENTED_EDGE('',*,*,#16171,.T.);
#22826=ORIENTED_EDGE('',*,*,#16172,.F.);
#22827=ORIENTED_EDGE('',*,*,#16171,.F.);
#22828=ORIENTED_EDGE('',*,*,#16165,.F.);
#22829=ORIENTED_EDGE('',*,*,#16173,.F.);
#22830=ORIENTED_EDGE('',*,*,#16174,.T.);
#22831=ORIENTED_EDGE('',*,*,#16175,.F.);
#22832=ORIENTED_EDGE('',*,*,#16176,.F.);
#22833=ORIENTED_EDGE('',*,*,#16177,.F.);
#22834=ORIENTED_EDGE('',*,*,#16176,.T.);
#22835=ORIENTED_EDGE('',*,*,#16178,.T.);
#22836=ORIENTED_EDGE('',*,*,#16179,.F.);
#22837=ORIENTED_EDGE('',*,*,#16178,.F.);
#22838=ORIENTED_EDGE('',*,*,#16175,.T.);
#22839=ORIENTED_EDGE('',*,*,#16180,.T.);
#22840=ORIENTED_EDGE('',*,*,#16181,.F.);
#22841=ORIENTED_EDGE('',*,*,#16180,.F.);
#22842=ORIENTED_EDGE('',*,*,#16174,.F.);
#22843=ORIENTED_EDGE('',*,*,#16182,.F.);
#22844=ORIENTED_EDGE('',*,*,#16183,.T.);
#22845=ORIENTED_EDGE('',*,*,#16184,.F.);
#22846=ORIENTED_EDGE('',*,*,#16185,.F.);
#22847=ORIENTED_EDGE('',*,*,#16186,.F.);
#22848=ORIENTED_EDGE('',*,*,#16185,.T.);
#22849=ORIENTED_EDGE('',*,*,#16187,.T.);
#22850=ORIENTED_EDGE('',*,*,#16188,.F.);
#22851=ORIENTED_EDGE('',*,*,#16187,.F.);
#22852=ORIENTED_EDGE('',*,*,#16184,.T.);
#22853=ORIENTED_EDGE('',*,*,#16189,.T.);
#22854=ORIENTED_EDGE('',*,*,#16190,.F.);
#22855=ORIENTED_EDGE('',*,*,#16189,.F.);
#22856=ORIENTED_EDGE('',*,*,#16183,.F.);
#22857=ORIENTED_EDGE('',*,*,#16191,.F.);
#22858=ORIENTED_EDGE('',*,*,#16192,.T.);
#22859=ORIENTED_EDGE('',*,*,#16193,.F.);
#22860=ORIENTED_EDGE('',*,*,#16194,.F.);
#22861=ORIENTED_EDGE('',*,*,#16195,.F.);
#22862=ORIENTED_EDGE('',*,*,#16194,.T.);
#22863=ORIENTED_EDGE('',*,*,#16196,.T.);
#22864=ORIENTED_EDGE('',*,*,#16197,.F.);
#22865=ORIENTED_EDGE('',*,*,#16196,.F.);
#22866=ORIENTED_EDGE('',*,*,#16193,.T.);
#22867=ORIENTED_EDGE('',*,*,#16198,.T.);
#22868=ORIENTED_EDGE('',*,*,#16199,.F.);
#22869=ORIENTED_EDGE('',*,*,#16198,.F.);
#22870=ORIENTED_EDGE('',*,*,#16192,.F.);
#22871=ORIENTED_EDGE('',*,*,#16200,.F.);
#22872=ORIENTED_EDGE('',*,*,#16201,.T.);
#22873=ORIENTED_EDGE('',*,*,#16202,.F.);
#22874=ORIENTED_EDGE('',*,*,#16203,.F.);
#22875=ORIENTED_EDGE('',*,*,#16204,.F.);
#22876=ORIENTED_EDGE('',*,*,#16203,.T.);
#22877=ORIENTED_EDGE('',*,*,#16205,.T.);
#22878=ORIENTED_EDGE('',*,*,#16206,.F.);
#22879=ORIENTED_EDGE('',*,*,#16205,.F.);
#22880=ORIENTED_EDGE('',*,*,#16202,.T.);
#22881=ORIENTED_EDGE('',*,*,#16207,.T.);
#22882=ORIENTED_EDGE('',*,*,#16208,.F.);
#22883=ORIENTED_EDGE('',*,*,#16207,.F.);
#22884=ORIENTED_EDGE('',*,*,#16201,.F.);
#22885=ORIENTED_EDGE('',*,*,#16209,.F.);
#22886=ORIENTED_EDGE('',*,*,#16210,.T.);
#22887=ORIENTED_EDGE('',*,*,#16211,.F.);
#22888=ORIENTED_EDGE('',*,*,#16212,.F.);
#22889=ORIENTED_EDGE('',*,*,#16213,.F.);
#22890=ORIENTED_EDGE('',*,*,#16212,.T.);
#22891=ORIENTED_EDGE('',*,*,#16214,.T.);
#22892=ORIENTED_EDGE('',*,*,#16215,.F.);
#22893=ORIENTED_EDGE('',*,*,#16214,.F.);
#22894=ORIENTED_EDGE('',*,*,#16211,.T.);
#22895=ORIENTED_EDGE('',*,*,#16216,.T.);
#22896=ORIENTED_EDGE('',*,*,#16217,.F.);
#22897=ORIENTED_EDGE('',*,*,#16216,.F.);
#22898=ORIENTED_EDGE('',*,*,#16210,.F.);
#22899=ORIENTED_EDGE('',*,*,#16218,.F.);
#22900=ORIENTED_EDGE('',*,*,#16219,.T.);
#22901=ORIENTED_EDGE('',*,*,#16220,.F.);
#22902=ORIENTED_EDGE('',*,*,#16221,.F.);
#22903=ORIENTED_EDGE('',*,*,#16222,.F.);
#22904=ORIENTED_EDGE('',*,*,#16221,.T.);
#22905=ORIENTED_EDGE('',*,*,#16223,.T.);
#22906=ORIENTED_EDGE('',*,*,#16224,.F.);
#22907=ORIENTED_EDGE('',*,*,#16223,.F.);
#22908=ORIENTED_EDGE('',*,*,#16220,.T.);
#22909=ORIENTED_EDGE('',*,*,#16225,.T.);
#22910=ORIENTED_EDGE('',*,*,#16226,.F.);
#22911=ORIENTED_EDGE('',*,*,#16225,.F.);
#22912=ORIENTED_EDGE('',*,*,#16219,.F.);
#22913=ORIENTED_EDGE('',*,*,#16227,.F.);
#22914=ORIENTED_EDGE('',*,*,#16228,.T.);
#22915=ORIENTED_EDGE('',*,*,#16229,.F.);
#22916=ORIENTED_EDGE('',*,*,#16230,.F.);
#22917=ORIENTED_EDGE('',*,*,#16231,.F.);
#22918=ORIENTED_EDGE('',*,*,#16230,.T.);
#22919=ORIENTED_EDGE('',*,*,#16232,.T.);
#22920=ORIENTED_EDGE('',*,*,#16233,.F.);
#22921=ORIENTED_EDGE('',*,*,#16232,.F.);
#22922=ORIENTED_EDGE('',*,*,#16229,.T.);
#22923=ORIENTED_EDGE('',*,*,#16234,.T.);
#22924=ORIENTED_EDGE('',*,*,#16235,.F.);
#22925=ORIENTED_EDGE('',*,*,#16234,.F.);
#22926=ORIENTED_EDGE('',*,*,#16228,.F.);
#22927=ORIENTED_EDGE('',*,*,#16236,.F.);
#22928=ORIENTED_EDGE('',*,*,#16237,.T.);
#22929=ORIENTED_EDGE('',*,*,#16238,.F.);
#22930=ORIENTED_EDGE('',*,*,#16239,.F.);
#22931=ORIENTED_EDGE('',*,*,#16240,.F.);
#22932=ORIENTED_EDGE('',*,*,#16239,.T.);
#22933=ORIENTED_EDGE('',*,*,#16241,.T.);
#22934=ORIENTED_EDGE('',*,*,#16242,.F.);
#22935=ORIENTED_EDGE('',*,*,#16241,.F.);
#22936=ORIENTED_EDGE('',*,*,#16238,.T.);
#22937=ORIENTED_EDGE('',*,*,#16243,.T.);
#22938=ORIENTED_EDGE('',*,*,#16244,.F.);
#22939=ORIENTED_EDGE('',*,*,#16243,.F.);
#22940=ORIENTED_EDGE('',*,*,#16237,.F.);
#22941=ORIENTED_EDGE('',*,*,#16245,.F.);
#22942=ORIENTED_EDGE('',*,*,#16246,.T.);
#22943=ORIENTED_EDGE('',*,*,#16247,.F.);
#22944=ORIENTED_EDGE('',*,*,#16248,.F.);
#22945=ORIENTED_EDGE('',*,*,#16249,.F.);
#22946=ORIENTED_EDGE('',*,*,#16248,.T.);
#22947=ORIENTED_EDGE('',*,*,#16250,.T.);
#22948=ORIENTED_EDGE('',*,*,#16251,.F.);
#22949=ORIENTED_EDGE('',*,*,#16250,.F.);
#22950=ORIENTED_EDGE('',*,*,#16247,.T.);
#22951=ORIENTED_EDGE('',*,*,#16252,.T.);
#22952=ORIENTED_EDGE('',*,*,#16253,.F.);
#22953=ORIENTED_EDGE('',*,*,#16252,.F.);
#22954=ORIENTED_EDGE('',*,*,#16246,.F.);
#22955=ORIENTED_EDGE('',*,*,#16254,.F.);
#22956=ORIENTED_EDGE('',*,*,#16255,.T.);
#22957=ORIENTED_EDGE('',*,*,#16256,.F.);
#22958=ORIENTED_EDGE('',*,*,#16257,.F.);
#22959=ORIENTED_EDGE('',*,*,#16258,.F.);
#22960=ORIENTED_EDGE('',*,*,#16257,.T.);
#22961=ORIENTED_EDGE('',*,*,#16259,.T.);
#22962=ORIENTED_EDGE('',*,*,#16260,.F.);
#22963=ORIENTED_EDGE('',*,*,#16259,.F.);
#22964=ORIENTED_EDGE('',*,*,#16256,.T.);
#22965=ORIENTED_EDGE('',*,*,#16261,.T.);
#22966=ORIENTED_EDGE('',*,*,#16262,.F.);
#22967=ORIENTED_EDGE('',*,*,#16261,.F.);
#22968=ORIENTED_EDGE('',*,*,#16255,.F.);
#22969=ORIENTED_EDGE('',*,*,#16263,.F.);
#22970=ORIENTED_EDGE('',*,*,#16264,.T.);
#22971=ORIENTED_EDGE('',*,*,#16265,.F.);
#22972=ORIENTED_EDGE('',*,*,#16266,.F.);
#22973=ORIENTED_EDGE('',*,*,#16267,.F.);
#22974=ORIENTED_EDGE('',*,*,#16266,.T.);
#22975=ORIENTED_EDGE('',*,*,#16268,.T.);
#22976=ORIENTED_EDGE('',*,*,#16269,.F.);
#22977=ORIENTED_EDGE('',*,*,#16268,.F.);
#22978=ORIENTED_EDGE('',*,*,#16265,.T.);
#22979=ORIENTED_EDGE('',*,*,#16270,.T.);
#22980=ORIENTED_EDGE('',*,*,#16271,.F.);
#22981=ORIENTED_EDGE('',*,*,#16270,.F.);
#22982=ORIENTED_EDGE('',*,*,#16264,.F.);
#22983=ORIENTED_EDGE('',*,*,#16272,.F.);
#22984=ORIENTED_EDGE('',*,*,#16273,.T.);
#22985=ORIENTED_EDGE('',*,*,#16274,.F.);
#22986=ORIENTED_EDGE('',*,*,#16275,.F.);
#22987=ORIENTED_EDGE('',*,*,#16276,.F.);
#22988=ORIENTED_EDGE('',*,*,#16275,.T.);
#22989=ORIENTED_EDGE('',*,*,#16277,.T.);
#22990=ORIENTED_EDGE('',*,*,#16278,.F.);
#22991=ORIENTED_EDGE('',*,*,#16277,.F.);
#22992=ORIENTED_EDGE('',*,*,#16274,.T.);
#22993=ORIENTED_EDGE('',*,*,#16279,.T.);
#22994=ORIENTED_EDGE('',*,*,#16280,.F.);
#22995=ORIENTED_EDGE('',*,*,#16279,.F.);
#22996=ORIENTED_EDGE('',*,*,#16273,.F.);
#22997=ORIENTED_EDGE('',*,*,#16281,.F.);
#22998=ORIENTED_EDGE('',*,*,#16282,.T.);
#22999=ORIENTED_EDGE('',*,*,#16283,.F.);
#23000=ORIENTED_EDGE('',*,*,#16284,.F.);
#23001=ORIENTED_EDGE('',*,*,#16285,.F.);
#23002=ORIENTED_EDGE('',*,*,#16284,.T.);
#23003=ORIENTED_EDGE('',*,*,#16286,.T.);
#23004=ORIENTED_EDGE('',*,*,#16287,.F.);
#23005=ORIENTED_EDGE('',*,*,#16286,.F.);
#23006=ORIENTED_EDGE('',*,*,#16283,.T.);
#23007=ORIENTED_EDGE('',*,*,#16288,.T.);
#23008=ORIENTED_EDGE('',*,*,#16289,.F.);
#23009=ORIENTED_EDGE('',*,*,#16288,.F.);
#23010=ORIENTED_EDGE('',*,*,#16282,.F.);
#23011=ORIENTED_EDGE('',*,*,#16290,.F.);
#23012=ORIENTED_EDGE('',*,*,#16291,.T.);
#23013=ORIENTED_EDGE('',*,*,#16292,.F.);
#23014=ORIENTED_EDGE('',*,*,#16293,.F.);
#23015=ORIENTED_EDGE('',*,*,#16294,.F.);
#23016=ORIENTED_EDGE('',*,*,#16293,.T.);
#23017=ORIENTED_EDGE('',*,*,#16295,.T.);
#23018=ORIENTED_EDGE('',*,*,#16296,.F.);
#23019=ORIENTED_EDGE('',*,*,#16295,.F.);
#23020=ORIENTED_EDGE('',*,*,#16292,.T.);
#23021=ORIENTED_EDGE('',*,*,#16297,.T.);
#23022=ORIENTED_EDGE('',*,*,#16298,.F.);
#23023=ORIENTED_EDGE('',*,*,#16297,.F.);
#23024=ORIENTED_EDGE('',*,*,#16291,.F.);
#23025=ORIENTED_EDGE('',*,*,#16299,.F.);
#23026=ORIENTED_EDGE('',*,*,#16300,.T.);
#23027=ORIENTED_EDGE('',*,*,#16301,.F.);
#23028=ORIENTED_EDGE('',*,*,#16302,.F.);
#23029=ORIENTED_EDGE('',*,*,#16303,.F.);
#23030=ORIENTED_EDGE('',*,*,#16302,.T.);
#23031=ORIENTED_EDGE('',*,*,#16304,.T.);
#23032=ORIENTED_EDGE('',*,*,#16305,.F.);
#23033=ORIENTED_EDGE('',*,*,#16304,.F.);
#23034=ORIENTED_EDGE('',*,*,#16301,.T.);
#23035=ORIENTED_EDGE('',*,*,#16306,.T.);
#23036=ORIENTED_EDGE('',*,*,#16307,.F.);
#23037=ORIENTED_EDGE('',*,*,#16306,.F.);
#23038=ORIENTED_EDGE('',*,*,#16300,.F.);
#23039=ORIENTED_EDGE('',*,*,#16308,.F.);
#23040=ORIENTED_EDGE('',*,*,#16309,.T.);
#23041=ORIENTED_EDGE('',*,*,#16310,.F.);
#23042=ORIENTED_EDGE('',*,*,#16311,.F.);
#23043=ORIENTED_EDGE('',*,*,#16312,.F.);
#23044=ORIENTED_EDGE('',*,*,#16311,.T.);
#23045=ORIENTED_EDGE('',*,*,#16313,.T.);
#23046=ORIENTED_EDGE('',*,*,#16314,.F.);
#23047=ORIENTED_EDGE('',*,*,#16313,.F.);
#23048=ORIENTED_EDGE('',*,*,#16310,.T.);
#23049=ORIENTED_EDGE('',*,*,#16315,.T.);
#23050=ORIENTED_EDGE('',*,*,#16316,.F.);
#23051=ORIENTED_EDGE('',*,*,#16315,.F.);
#23052=ORIENTED_EDGE('',*,*,#16309,.F.);
#23053=ORIENTED_EDGE('',*,*,#16317,.F.);
#23054=ORIENTED_EDGE('',*,*,#16318,.T.);
#23055=ORIENTED_EDGE('',*,*,#16319,.F.);
#23056=ORIENTED_EDGE('',*,*,#16320,.F.);
#23057=ORIENTED_EDGE('',*,*,#16321,.F.);
#23058=ORIENTED_EDGE('',*,*,#16320,.T.);
#23059=ORIENTED_EDGE('',*,*,#16322,.T.);
#23060=ORIENTED_EDGE('',*,*,#16323,.F.);
#23061=ORIENTED_EDGE('',*,*,#16324,.F.);
#23062=ORIENTED_EDGE('',*,*,#16322,.F.);
#23063=ORIENTED_EDGE('',*,*,#16319,.T.);
#23064=ORIENTED_EDGE('',*,*,#16325,.T.);
#23065=ORIENTED_EDGE('',*,*,#16326,.F.);
#23066=ORIENTED_EDGE('',*,*,#16325,.F.);
#23067=ORIENTED_EDGE('',*,*,#16318,.F.);
#23068=ORIENTED_EDGE('',*,*,#16327,.F.);
#23069=ORIENTED_EDGE('',*,*,#16328,.F.);
#23070=ORIENTED_EDGE('',*,*,#16329,.T.);
#23071=ORIENTED_EDGE('',*,*,#16330,.F.);
#23072=ORIENTED_EDGE('',*,*,#16331,.F.);
#23073=ORIENTED_EDGE('',*,*,#16332,.F.);
#23074=ORIENTED_EDGE('',*,*,#16331,.T.);
#23075=ORIENTED_EDGE('',*,*,#16333,.T.);
#23076=ORIENTED_EDGE('',*,*,#16334,.F.);
#23077=ORIENTED_EDGE('',*,*,#16333,.F.);
#23078=ORIENTED_EDGE('',*,*,#16330,.T.);
#23079=ORIENTED_EDGE('',*,*,#16335,.T.);
#23080=ORIENTED_EDGE('',*,*,#16336,.F.);
#23081=ORIENTED_EDGE('',*,*,#16335,.F.);
#23082=ORIENTED_EDGE('',*,*,#16329,.F.);
#23083=ORIENTED_EDGE('',*,*,#16337,.F.);
#23084=ORIENTED_EDGE('',*,*,#16338,.T.);
#23085=ORIENTED_EDGE('',*,*,#16339,.F.);
#23086=ORIENTED_EDGE('',*,*,#16340,.F.);
#23087=ORIENTED_EDGE('',*,*,#16341,.F.);
#23088=ORIENTED_EDGE('',*,*,#16340,.T.);
#23089=ORIENTED_EDGE('',*,*,#16342,.T.);
#23090=ORIENTED_EDGE('',*,*,#16343,.F.);
#23091=ORIENTED_EDGE('',*,*,#16342,.F.);
#23092=ORIENTED_EDGE('',*,*,#16339,.T.);
#23093=ORIENTED_EDGE('',*,*,#16344,.T.);
#23094=ORIENTED_EDGE('',*,*,#16345,.F.);
#23095=ORIENTED_EDGE('',*,*,#16344,.F.);
#23096=ORIENTED_EDGE('',*,*,#16338,.F.);
#23097=ORIENTED_EDGE('',*,*,#16346,.F.);
#23098=ORIENTED_EDGE('',*,*,#16347,.T.);
#23099=ORIENTED_EDGE('',*,*,#16348,.F.);
#23100=ORIENTED_EDGE('',*,*,#16349,.F.);
#23101=ORIENTED_EDGE('',*,*,#16350,.F.);
#23102=ORIENTED_EDGE('',*,*,#16349,.T.);
#23103=ORIENTED_EDGE('',*,*,#16351,.T.);
#23104=ORIENTED_EDGE('',*,*,#16352,.F.);
#23105=ORIENTED_EDGE('',*,*,#16351,.F.);
#23106=ORIENTED_EDGE('',*,*,#16348,.T.);
#23107=ORIENTED_EDGE('',*,*,#16353,.T.);
#23108=ORIENTED_EDGE('',*,*,#16354,.F.);
#23109=ORIENTED_EDGE('',*,*,#16353,.F.);
#23110=ORIENTED_EDGE('',*,*,#16347,.F.);
#23111=ORIENTED_EDGE('',*,*,#16355,.F.);
#23112=ORIENTED_EDGE('',*,*,#16356,.T.);
#23113=ORIENTED_EDGE('',*,*,#16357,.F.);
#23114=ORIENTED_EDGE('',*,*,#16358,.F.);
#23115=ORIENTED_EDGE('',*,*,#16359,.F.);
#23116=ORIENTED_EDGE('',*,*,#16358,.T.);
#23117=ORIENTED_EDGE('',*,*,#16360,.T.);
#23118=ORIENTED_EDGE('',*,*,#16361,.F.);
#23119=ORIENTED_EDGE('',*,*,#16360,.F.);
#23120=ORIENTED_EDGE('',*,*,#16357,.T.);
#23121=ORIENTED_EDGE('',*,*,#16362,.T.);
#23122=ORIENTED_EDGE('',*,*,#16363,.F.);
#23123=ORIENTED_EDGE('',*,*,#16362,.F.);
#23124=ORIENTED_EDGE('',*,*,#16356,.F.);
#23125=ORIENTED_EDGE('',*,*,#16364,.F.);
#23126=ORIENTED_EDGE('',*,*,#16365,.T.);
#23127=ORIENTED_EDGE('',*,*,#16366,.F.);
#23128=ORIENTED_EDGE('',*,*,#16367,.F.);
#23129=ORIENTED_EDGE('',*,*,#16368,.F.);
#23130=ORIENTED_EDGE('',*,*,#16367,.T.);
#23131=ORIENTED_EDGE('',*,*,#16369,.T.);
#23132=ORIENTED_EDGE('',*,*,#16370,.F.);
#23133=ORIENTED_EDGE('',*,*,#16369,.F.);
#23134=ORIENTED_EDGE('',*,*,#16366,.T.);
#23135=ORIENTED_EDGE('',*,*,#16371,.T.);
#23136=ORIENTED_EDGE('',*,*,#16372,.F.);
#23137=ORIENTED_EDGE('',*,*,#16371,.F.);
#23138=ORIENTED_EDGE('',*,*,#16365,.F.);
#23139=ORIENTED_EDGE('',*,*,#16373,.F.);
#23140=ORIENTED_EDGE('',*,*,#16374,.T.);
#23141=ORIENTED_EDGE('',*,*,#16375,.F.);
#23142=ORIENTED_EDGE('',*,*,#16376,.F.);
#23143=ORIENTED_EDGE('',*,*,#16377,.F.);
#23144=ORIENTED_EDGE('',*,*,#16376,.T.);
#23145=ORIENTED_EDGE('',*,*,#16378,.T.);
#23146=ORIENTED_EDGE('',*,*,#16379,.F.);
#23147=ORIENTED_EDGE('',*,*,#16378,.F.);
#23148=ORIENTED_EDGE('',*,*,#16375,.T.);
#23149=ORIENTED_EDGE('',*,*,#16380,.T.);
#23150=ORIENTED_EDGE('',*,*,#16381,.F.);
#23151=ORIENTED_EDGE('',*,*,#16380,.F.);
#23152=ORIENTED_EDGE('',*,*,#16374,.F.);
#23153=ORIENTED_EDGE('',*,*,#16382,.F.);
#23154=ORIENTED_EDGE('',*,*,#16383,.T.);
#23155=ORIENTED_EDGE('',*,*,#16384,.F.);
#23156=ORIENTED_EDGE('',*,*,#16385,.F.);
#23157=ORIENTED_EDGE('',*,*,#16386,.F.);
#23158=ORIENTED_EDGE('',*,*,#16385,.T.);
#23159=ORIENTED_EDGE('',*,*,#16387,.T.);
#23160=ORIENTED_EDGE('',*,*,#16388,.F.);
#23161=ORIENTED_EDGE('',*,*,#16387,.F.);
#23162=ORIENTED_EDGE('',*,*,#16384,.T.);
#23163=ORIENTED_EDGE('',*,*,#16389,.T.);
#23164=ORIENTED_EDGE('',*,*,#16390,.F.);
#23165=ORIENTED_EDGE('',*,*,#16389,.F.);
#23166=ORIENTED_EDGE('',*,*,#16383,.F.);
#23167=ORIENTED_EDGE('',*,*,#16391,.F.);
#23168=ORIENTED_EDGE('',*,*,#16392,.T.);
#23169=ORIENTED_EDGE('',*,*,#16393,.F.);
#23170=ORIENTED_EDGE('',*,*,#16394,.F.);
#23171=ORIENTED_EDGE('',*,*,#16395,.F.);
#23172=ORIENTED_EDGE('',*,*,#16394,.T.);
#23173=ORIENTED_EDGE('',*,*,#16396,.T.);
#23174=ORIENTED_EDGE('',*,*,#16397,.F.);
#23175=ORIENTED_EDGE('',*,*,#16396,.F.);
#23176=ORIENTED_EDGE('',*,*,#16393,.T.);
#23177=ORIENTED_EDGE('',*,*,#16398,.T.);
#23178=ORIENTED_EDGE('',*,*,#16399,.F.);
#23179=ORIENTED_EDGE('',*,*,#16398,.F.);
#23180=ORIENTED_EDGE('',*,*,#16392,.F.);
#23181=ORIENTED_EDGE('',*,*,#16400,.F.);
#23182=ORIENTED_EDGE('',*,*,#16401,.T.);
#23183=ORIENTED_EDGE('',*,*,#16402,.F.);
#23184=ORIENTED_EDGE('',*,*,#16403,.F.);
#23185=ORIENTED_EDGE('',*,*,#16404,.F.);
#23186=ORIENTED_EDGE('',*,*,#16403,.T.);
#23187=ORIENTED_EDGE('',*,*,#16405,.T.);
#23188=ORIENTED_EDGE('',*,*,#16406,.F.);
#23189=ORIENTED_EDGE('',*,*,#16405,.F.);
#23190=ORIENTED_EDGE('',*,*,#16402,.T.);
#23191=ORIENTED_EDGE('',*,*,#16407,.T.);
#23192=ORIENTED_EDGE('',*,*,#16408,.F.);
#23193=ORIENTED_EDGE('',*,*,#16407,.F.);
#23194=ORIENTED_EDGE('',*,*,#16401,.F.);
#23195=ORIENTED_EDGE('',*,*,#16409,.F.);
#23196=ORIENTED_EDGE('',*,*,#16410,.T.);
#23197=ORIENTED_EDGE('',*,*,#16411,.F.);
#23198=ORIENTED_EDGE('',*,*,#16412,.F.);
#23199=ORIENTED_EDGE('',*,*,#16413,.F.);
#23200=ORIENTED_EDGE('',*,*,#16412,.T.);
#23201=ORIENTED_EDGE('',*,*,#16414,.T.);
#23202=ORIENTED_EDGE('',*,*,#16415,.F.);
#23203=ORIENTED_EDGE('',*,*,#16414,.F.);
#23204=ORIENTED_EDGE('',*,*,#16411,.T.);
#23205=ORIENTED_EDGE('',*,*,#16416,.T.);
#23206=ORIENTED_EDGE('',*,*,#16417,.F.);
#23207=ORIENTED_EDGE('',*,*,#16416,.F.);
#23208=ORIENTED_EDGE('',*,*,#16410,.F.);
#23209=ORIENTED_EDGE('',*,*,#16418,.F.);
#23210=ORIENTED_EDGE('',*,*,#16419,.T.);
#23211=ORIENTED_EDGE('',*,*,#16420,.F.);
#23212=ORIENTED_EDGE('',*,*,#16421,.F.);
#23213=ORIENTED_EDGE('',*,*,#16422,.F.);
#23214=ORIENTED_EDGE('',*,*,#16421,.T.);
#23215=ORIENTED_EDGE('',*,*,#16423,.T.);
#23216=ORIENTED_EDGE('',*,*,#16424,.F.);
#23217=ORIENTED_EDGE('',*,*,#16423,.F.);
#23218=ORIENTED_EDGE('',*,*,#16420,.T.);
#23219=ORIENTED_EDGE('',*,*,#16425,.T.);
#23220=ORIENTED_EDGE('',*,*,#16426,.F.);
#23221=ORIENTED_EDGE('',*,*,#16425,.F.);
#23222=ORIENTED_EDGE('',*,*,#16419,.F.);
#23223=ORIENTED_EDGE('',*,*,#16427,.F.);
#23224=ORIENTED_EDGE('',*,*,#16428,.T.);
#23225=ORIENTED_EDGE('',*,*,#16429,.F.);
#23226=ORIENTED_EDGE('',*,*,#16430,.F.);
#23227=ORIENTED_EDGE('',*,*,#16431,.F.);
#23228=ORIENTED_EDGE('',*,*,#16430,.T.);
#23229=ORIENTED_EDGE('',*,*,#16432,.T.);
#23230=ORIENTED_EDGE('',*,*,#16433,.F.);
#23231=ORIENTED_EDGE('',*,*,#16432,.F.);
#23232=ORIENTED_EDGE('',*,*,#16429,.T.);
#23233=ORIENTED_EDGE('',*,*,#16434,.T.);
#23234=ORIENTED_EDGE('',*,*,#16435,.F.);
#23235=ORIENTED_EDGE('',*,*,#16434,.F.);
#23236=ORIENTED_EDGE('',*,*,#16428,.F.);
#23237=ORIENTED_EDGE('',*,*,#16436,.F.);
#23238=ORIENTED_EDGE('',*,*,#16437,.T.);
#23239=ORIENTED_EDGE('',*,*,#16438,.F.);
#23240=ORIENTED_EDGE('',*,*,#16439,.F.);
#23241=ORIENTED_EDGE('',*,*,#16440,.F.);
#23242=ORIENTED_EDGE('',*,*,#16439,.T.);
#23243=ORIENTED_EDGE('',*,*,#16441,.T.);
#23244=ORIENTED_EDGE('',*,*,#16442,.F.);
#23245=ORIENTED_EDGE('',*,*,#16441,.F.);
#23246=ORIENTED_EDGE('',*,*,#16438,.T.);
#23247=ORIENTED_EDGE('',*,*,#16443,.T.);
#23248=ORIENTED_EDGE('',*,*,#16444,.F.);
#23249=ORIENTED_EDGE('',*,*,#16443,.F.);
#23250=ORIENTED_EDGE('',*,*,#16437,.F.);
#23251=ORIENTED_EDGE('',*,*,#16445,.F.);
#23252=ORIENTED_EDGE('',*,*,#16446,.T.);
#23253=ORIENTED_EDGE('',*,*,#16447,.F.);
#23254=ORIENTED_EDGE('',*,*,#16448,.F.);
#23255=ORIENTED_EDGE('',*,*,#16449,.F.);
#23256=ORIENTED_EDGE('',*,*,#16448,.T.);
#23257=ORIENTED_EDGE('',*,*,#16450,.T.);
#23258=ORIENTED_EDGE('',*,*,#16451,.F.);
#23259=ORIENTED_EDGE('',*,*,#16450,.F.);
#23260=ORIENTED_EDGE('',*,*,#16447,.T.);
#23261=ORIENTED_EDGE('',*,*,#16452,.T.);
#23262=ORIENTED_EDGE('',*,*,#16453,.F.);
#23263=ORIENTED_EDGE('',*,*,#16452,.F.);
#23264=ORIENTED_EDGE('',*,*,#16446,.F.);
#23265=ORIENTED_EDGE('',*,*,#16454,.F.);
#23266=ORIENTED_EDGE('',*,*,#16455,.T.);
#23267=ORIENTED_EDGE('',*,*,#16456,.F.);
#23268=ORIENTED_EDGE('',*,*,#16457,.F.);
#23269=ORIENTED_EDGE('',*,*,#16458,.F.);
#23270=ORIENTED_EDGE('',*,*,#16457,.T.);
#23271=ORIENTED_EDGE('',*,*,#16459,.T.);
#23272=ORIENTED_EDGE('',*,*,#16460,.F.);
#23273=ORIENTED_EDGE('',*,*,#16459,.F.);
#23274=ORIENTED_EDGE('',*,*,#16456,.T.);
#23275=ORIENTED_EDGE('',*,*,#16461,.T.);
#23276=ORIENTED_EDGE('',*,*,#16462,.F.);
#23277=ORIENTED_EDGE('',*,*,#16461,.F.);
#23278=ORIENTED_EDGE('',*,*,#16455,.F.);
#23279=ORIENTED_EDGE('',*,*,#16463,.F.);
#23280=ORIENTED_EDGE('',*,*,#16464,.T.);
#23281=ORIENTED_EDGE('',*,*,#16465,.F.);
#23282=ORIENTED_EDGE('',*,*,#16466,.F.);
#23283=ORIENTED_EDGE('',*,*,#16467,.F.);
#23284=ORIENTED_EDGE('',*,*,#16466,.T.);
#23285=ORIENTED_EDGE('',*,*,#16468,.T.);
#23286=ORIENTED_EDGE('',*,*,#16469,.F.);
#23287=ORIENTED_EDGE('',*,*,#16468,.F.);
#23288=ORIENTED_EDGE('',*,*,#16465,.T.);
#23289=ORIENTED_EDGE('',*,*,#16470,.T.);
#23290=ORIENTED_EDGE('',*,*,#16471,.F.);
#23291=ORIENTED_EDGE('',*,*,#16470,.F.);
#23292=ORIENTED_EDGE('',*,*,#16464,.F.);
#23293=ORIENTED_EDGE('',*,*,#16472,.F.);
#23294=ORIENTED_EDGE('',*,*,#16473,.T.);
#23295=ORIENTED_EDGE('',*,*,#16474,.F.);
#23296=ORIENTED_EDGE('',*,*,#16475,.F.);
#23297=ORIENTED_EDGE('',*,*,#16476,.F.);
#23298=ORIENTED_EDGE('',*,*,#16475,.T.);
#23299=ORIENTED_EDGE('',*,*,#16477,.T.);
#23300=ORIENTED_EDGE('',*,*,#16478,.F.);
#23301=ORIENTED_EDGE('',*,*,#16477,.F.);
#23302=ORIENTED_EDGE('',*,*,#16474,.T.);
#23303=ORIENTED_EDGE('',*,*,#16479,.T.);
#23304=ORIENTED_EDGE('',*,*,#16480,.F.);
#23305=ORIENTED_EDGE('',*,*,#16479,.F.);
#23306=ORIENTED_EDGE('',*,*,#16473,.F.);
#23307=ORIENTED_EDGE('',*,*,#16481,.F.);
#23308=ORIENTED_EDGE('',*,*,#16482,.T.);
#23309=ORIENTED_EDGE('',*,*,#16483,.F.);
#23310=ORIENTED_EDGE('',*,*,#16484,.F.);
#23311=ORIENTED_EDGE('',*,*,#16485,.F.);
#23312=ORIENTED_EDGE('',*,*,#16484,.T.);
#23313=ORIENTED_EDGE('',*,*,#16486,.T.);
#23314=ORIENTED_EDGE('',*,*,#16487,.F.);
#23315=ORIENTED_EDGE('',*,*,#16486,.F.);
#23316=ORIENTED_EDGE('',*,*,#16483,.T.);
#23317=ORIENTED_EDGE('',*,*,#16488,.T.);
#23318=ORIENTED_EDGE('',*,*,#16489,.F.);
#23319=ORIENTED_EDGE('',*,*,#16488,.F.);
#23320=ORIENTED_EDGE('',*,*,#16482,.F.);
#23321=ORIENTED_EDGE('',*,*,#16490,.F.);
#23322=ORIENTED_EDGE('',*,*,#16491,.T.);
#23323=ORIENTED_EDGE('',*,*,#16492,.T.);
#23324=ORIENTED_EDGE('',*,*,#16493,.F.);
#23325=ORIENTED_EDGE('',*,*,#16494,.F.);
#23326=ORIENTED_EDGE('',*,*,#16495,.T.);
#23327=ORIENTED_EDGE('',*,*,#16496,.T.);
#23328=ORIENTED_EDGE('',*,*,#16491,.F.);
#23329=ORIENTED_EDGE('',*,*,#16497,.F.);
#23330=ORIENTED_EDGE('',*,*,#16498,.T.);
#23331=ORIENTED_EDGE('',*,*,#16499,.T.);
#23332=ORIENTED_EDGE('',*,*,#16495,.F.);
#23333=ORIENTED_EDGE('',*,*,#16500,.F.);
#23334=ORIENTED_EDGE('',*,*,#16501,.T.);
#23335=ORIENTED_EDGE('',*,*,#16502,.T.);
#23336=ORIENTED_EDGE('',*,*,#16498,.F.);
#23337=ORIENTED_EDGE('',*,*,#16503,.F.);
#23338=ORIENTED_EDGE('',*,*,#16504,.T.);
#23339=ORIENTED_EDGE('',*,*,#16505,.T.);
#23340=ORIENTED_EDGE('',*,*,#16501,.F.);
#23341=ORIENTED_EDGE('',*,*,#16506,.F.);
#23342=ORIENTED_EDGE('',*,*,#16493,.T.);
#23343=ORIENTED_EDGE('',*,*,#16507,.T.);
#23344=ORIENTED_EDGE('',*,*,#16504,.F.);
#23345=ORIENTED_EDGE('',*,*,#16507,.F.);
#23346=ORIENTED_EDGE('',*,*,#16492,.F.);
#23347=ORIENTED_EDGE('',*,*,#16496,.F.);
#23348=ORIENTED_EDGE('',*,*,#16499,.F.);
#23349=ORIENTED_EDGE('',*,*,#16502,.F.);
#23350=ORIENTED_EDGE('',*,*,#16505,.F.);
#23351=ORIENTED_EDGE('',*,*,#16508,.F.);
#23352=ORIENTED_EDGE('',*,*,#16159,.F.);
#23353=ORIENTED_EDGE('',*,*,#16029,.F.);
#23354=ORIENTED_EDGE('',*,*,#16160,.F.);
#23355=ORIENTED_EDGE('',*,*,#16509,.T.);
#23356=ORIENTED_EDGE('',*,*,#16508,.T.);
#23357=ORIENTED_EDGE('',*,*,#16509,.F.);
#23358=ORIENTED_EDGE('',*,*,#16088,.T.);
#23359=ORIENTED_EDGE('',*,*,#16156,.T.);
#23360=ORIENTED_EDGE('',*,*,#16510,.F.);
#23361=ORIENTED_EDGE('',*,*,#16511,.F.);
#23362=ORIENTED_EDGE('',*,*,#16512,.T.);
#23363=ORIENTED_EDGE('',*,*,#16510,.T.);
#23364=ORIENTED_EDGE('',*,*,#16154,.T.);
#23365=ORIENTED_EDGE('',*,*,#16089,.T.);
#23366=ORIENTED_EDGE('',*,*,#16512,.F.);
#23367=ORIENTED_EDGE('',*,*,#16513,.F.);
#23368=ORIENTED_EDGE('',*,*,#16514,.T.);
#23369=ORIENTED_EDGE('',*,*,#16511,.T.);
#23370=ORIENTED_EDGE('',*,*,#16514,.F.);
#23371=ORIENTED_EDGE('',*,*,#16515,.F.);
#23372=ORIENTED_EDGE('',*,*,#16513,.T.);
#23373=ORIENTED_EDGE('',*,*,#16516,.F.);
#23374=ORIENTED_EDGE('',*,*,#16517,.T.);
#23375=ORIENTED_EDGE('',*,*,#16327,.T.);
#23376=ORIENTED_EDGE('',*,*,#16317,.T.);
#23377=ORIENTED_EDGE('',*,*,#16321,.T.);
#23378=ORIENTED_EDGE('',*,*,#16518,.T.);
#23379=ORIENTED_EDGE('',*,*,#16515,.T.);
#23380=ORIENTED_EDGE('',*,*,#16518,.F.);
#23381=ORIENTED_EDGE('',*,*,#16323,.T.);
#23382=ORIENTED_EDGE('',*,*,#16324,.T.);
#23383=ORIENTED_EDGE('',*,*,#16326,.T.);
#23384=ORIENTED_EDGE('',*,*,#16517,.F.);
#23385=ORIENTED_EDGE('',*,*,#16170,.T.);
#23386=ORIENTED_EDGE('',*,*,#16172,.T.);
#23387=ORIENTED_EDGE('',*,*,#16164,.T.);
#23388=ORIENTED_EDGE('',*,*,#16168,.T.);
#23389=ORIENTED_EDGE('',*,*,#16179,.T.);
#23390=ORIENTED_EDGE('',*,*,#16181,.T.);
#23391=ORIENTED_EDGE('',*,*,#16173,.T.);
#23392=ORIENTED_EDGE('',*,*,#16177,.T.);
#23393=ORIENTED_EDGE('',*,*,#16188,.T.);
#23394=ORIENTED_EDGE('',*,*,#16190,.T.);
#23395=ORIENTED_EDGE('',*,*,#16182,.T.);
#23396=ORIENTED_EDGE('',*,*,#16186,.T.);
#23397=ORIENTED_EDGE('',*,*,#16197,.T.);
#23398=ORIENTED_EDGE('',*,*,#16199,.T.);
#23399=ORIENTED_EDGE('',*,*,#16191,.T.);
#23400=ORIENTED_EDGE('',*,*,#16195,.T.);
#23401=ORIENTED_EDGE('',*,*,#16206,.T.);
#23402=ORIENTED_EDGE('',*,*,#16208,.T.);
#23403=ORIENTED_EDGE('',*,*,#16200,.T.);
#23404=ORIENTED_EDGE('',*,*,#16204,.T.);
#23405=ORIENTED_EDGE('',*,*,#16215,.T.);
#23406=ORIENTED_EDGE('',*,*,#16217,.T.);
#23407=ORIENTED_EDGE('',*,*,#16209,.T.);
#23408=ORIENTED_EDGE('',*,*,#16213,.T.);
#23409=ORIENTED_EDGE('',*,*,#16224,.T.);
#23410=ORIENTED_EDGE('',*,*,#16226,.T.);
#23411=ORIENTED_EDGE('',*,*,#16218,.T.);
#23412=ORIENTED_EDGE('',*,*,#16222,.T.);
#23413=ORIENTED_EDGE('',*,*,#16233,.T.);
#23414=ORIENTED_EDGE('',*,*,#16235,.T.);
#23415=ORIENTED_EDGE('',*,*,#16227,.T.);
#23416=ORIENTED_EDGE('',*,*,#16231,.T.);
#23417=ORIENTED_EDGE('',*,*,#16242,.T.);
#23418=ORIENTED_EDGE('',*,*,#16244,.T.);
#23419=ORIENTED_EDGE('',*,*,#16236,.T.);
#23420=ORIENTED_EDGE('',*,*,#16240,.T.);
#23421=ORIENTED_EDGE('',*,*,#16251,.T.);
#23422=ORIENTED_EDGE('',*,*,#16253,.T.);
#23423=ORIENTED_EDGE('',*,*,#16245,.T.);
#23424=ORIENTED_EDGE('',*,*,#16249,.T.);
#23425=ORIENTED_EDGE('',*,*,#16260,.T.);
#23426=ORIENTED_EDGE('',*,*,#16262,.T.);
#23427=ORIENTED_EDGE('',*,*,#16254,.T.);
#23428=ORIENTED_EDGE('',*,*,#16258,.T.);
#23429=ORIENTED_EDGE('',*,*,#16269,.T.);
#23430=ORIENTED_EDGE('',*,*,#16271,.T.);
#23431=ORIENTED_EDGE('',*,*,#16263,.T.);
#23432=ORIENTED_EDGE('',*,*,#16267,.T.);
#23433=ORIENTED_EDGE('',*,*,#16278,.T.);
#23434=ORIENTED_EDGE('',*,*,#16280,.T.);
#23435=ORIENTED_EDGE('',*,*,#16272,.T.);
#23436=ORIENTED_EDGE('',*,*,#16276,.T.);
#23437=ORIENTED_EDGE('',*,*,#16287,.T.);
#23438=ORIENTED_EDGE('',*,*,#16289,.T.);
#23439=ORIENTED_EDGE('',*,*,#16281,.T.);
#23440=ORIENTED_EDGE('',*,*,#16285,.T.);
#23441=ORIENTED_EDGE('',*,*,#16296,.T.);
#23442=ORIENTED_EDGE('',*,*,#16298,.T.);
#23443=ORIENTED_EDGE('',*,*,#16290,.T.);
#23444=ORIENTED_EDGE('',*,*,#16294,.T.);
#23445=ORIENTED_EDGE('',*,*,#16305,.T.);
#23446=ORIENTED_EDGE('',*,*,#16307,.T.);
#23447=ORIENTED_EDGE('',*,*,#16299,.T.);
#23448=ORIENTED_EDGE('',*,*,#16303,.T.);
#23449=ORIENTED_EDGE('',*,*,#16314,.T.);
#23450=ORIENTED_EDGE('',*,*,#16316,.T.);
#23451=ORIENTED_EDGE('',*,*,#16308,.T.);
#23452=ORIENTED_EDGE('',*,*,#16312,.T.);
#23453=ORIENTED_EDGE('',*,*,#16334,.T.);
#23454=ORIENTED_EDGE('',*,*,#16336,.T.);
#23455=ORIENTED_EDGE('',*,*,#16328,.T.);
#23456=ORIENTED_EDGE('',*,*,#16332,.T.);
#23457=ORIENTED_EDGE('',*,*,#16343,.T.);
#23458=ORIENTED_EDGE('',*,*,#16345,.T.);
#23459=ORIENTED_EDGE('',*,*,#16337,.T.);
#23460=ORIENTED_EDGE('',*,*,#16341,.T.);
#23461=ORIENTED_EDGE('',*,*,#16352,.T.);
#23462=ORIENTED_EDGE('',*,*,#16354,.T.);
#23463=ORIENTED_EDGE('',*,*,#16346,.T.);
#23464=ORIENTED_EDGE('',*,*,#16350,.T.);
#23465=ORIENTED_EDGE('',*,*,#16361,.T.);
#23466=ORIENTED_EDGE('',*,*,#16363,.T.);
#23467=ORIENTED_EDGE('',*,*,#16355,.T.);
#23468=ORIENTED_EDGE('',*,*,#16359,.T.);
#23469=ORIENTED_EDGE('',*,*,#16370,.T.);
#23470=ORIENTED_EDGE('',*,*,#16372,.T.);
#23471=ORIENTED_EDGE('',*,*,#16364,.T.);
#23472=ORIENTED_EDGE('',*,*,#16368,.T.);
#23473=ORIENTED_EDGE('',*,*,#16379,.T.);
#23474=ORIENTED_EDGE('',*,*,#16381,.T.);
#23475=ORIENTED_EDGE('',*,*,#16373,.T.);
#23476=ORIENTED_EDGE('',*,*,#16377,.T.);
#23477=ORIENTED_EDGE('',*,*,#16388,.T.);
#23478=ORIENTED_EDGE('',*,*,#16390,.T.);
#23479=ORIENTED_EDGE('',*,*,#16382,.T.);
#23480=ORIENTED_EDGE('',*,*,#16386,.T.);
#23481=ORIENTED_EDGE('',*,*,#16397,.T.);
#23482=ORIENTED_EDGE('',*,*,#16399,.T.);
#23483=ORIENTED_EDGE('',*,*,#16391,.T.);
#23484=ORIENTED_EDGE('',*,*,#16395,.T.);
#23485=ORIENTED_EDGE('',*,*,#16406,.T.);
#23486=ORIENTED_EDGE('',*,*,#16408,.T.);
#23487=ORIENTED_EDGE('',*,*,#16400,.T.);
#23488=ORIENTED_EDGE('',*,*,#16404,.T.);
#23489=ORIENTED_EDGE('',*,*,#16415,.T.);
#23490=ORIENTED_EDGE('',*,*,#16417,.T.);
#23491=ORIENTED_EDGE('',*,*,#16409,.T.);
#23492=ORIENTED_EDGE('',*,*,#16413,.T.);
#23493=ORIENTED_EDGE('',*,*,#16424,.T.);
#23494=ORIENTED_EDGE('',*,*,#16426,.T.);
#23495=ORIENTED_EDGE('',*,*,#16418,.T.);
#23496=ORIENTED_EDGE('',*,*,#16422,.T.);
#23497=ORIENTED_EDGE('',*,*,#16433,.T.);
#23498=ORIENTED_EDGE('',*,*,#16435,.T.);
#23499=ORIENTED_EDGE('',*,*,#16427,.T.);
#23500=ORIENTED_EDGE('',*,*,#16431,.T.);
#23501=ORIENTED_EDGE('',*,*,#16442,.T.);
#23502=ORIENTED_EDGE('',*,*,#16444,.T.);
#23503=ORIENTED_EDGE('',*,*,#16436,.T.);
#23504=ORIENTED_EDGE('',*,*,#16440,.T.);
#23505=ORIENTED_EDGE('',*,*,#16451,.T.);
#23506=ORIENTED_EDGE('',*,*,#16453,.T.);
#23507=ORIENTED_EDGE('',*,*,#16445,.T.);
#23508=ORIENTED_EDGE('',*,*,#16449,.T.);
#23509=ORIENTED_EDGE('',*,*,#16460,.T.);
#23510=ORIENTED_EDGE('',*,*,#16462,.T.);
#23511=ORIENTED_EDGE('',*,*,#16454,.T.);
#23512=ORIENTED_EDGE('',*,*,#16458,.T.);
#23513=ORIENTED_EDGE('',*,*,#16469,.T.);
#23514=ORIENTED_EDGE('',*,*,#16471,.T.);
#23515=ORIENTED_EDGE('',*,*,#16463,.T.);
#23516=ORIENTED_EDGE('',*,*,#16467,.T.);
#23517=ORIENTED_EDGE('',*,*,#16478,.T.);
#23518=ORIENTED_EDGE('',*,*,#16480,.T.);
#23519=ORIENTED_EDGE('',*,*,#16472,.T.);
#23520=ORIENTED_EDGE('',*,*,#16476,.T.);
#23521=ORIENTED_EDGE('',*,*,#16487,.T.);
#23522=ORIENTED_EDGE('',*,*,#16489,.T.);
#23523=ORIENTED_EDGE('',*,*,#16481,.T.);
#23524=ORIENTED_EDGE('',*,*,#16485,.T.);
#23525=ORIENTED_EDGE('',*,*,#16519,.F.);
#23526=ORIENTED_EDGE('',*,*,#16520,.T.);
#23527=ORIENTED_EDGE('',*,*,#16516,.T.);
#23528=ORIENTED_EDGE('',*,*,#16520,.F.);
#23529=ORIENTED_EDGE('',*,*,#16519,.T.);
#23530=ORIENTED_EDGE('',*,*,#16490,.T.);
#23531=ORIENTED_EDGE('',*,*,#16506,.T.);
#23532=ORIENTED_EDGE('',*,*,#16503,.T.);
#23533=ORIENTED_EDGE('',*,*,#16500,.T.);
#23534=ORIENTED_EDGE('',*,*,#16497,.T.);
#23535=ORIENTED_EDGE('',*,*,#16494,.T.);
#23536=ORIENTED_EDGE('',*,*,#16521,.F.);
#23537=ORIENTED_EDGE('',*,*,#16522,.F.);
#23538=ORIENTED_EDGE('',*,*,#16523,.T.);
#23539=ORIENTED_EDGE('',*,*,#16521,.T.);
#23540=ORIENTED_EDGE('',*,*,#16523,.F.);
#23541=ORIENTED_EDGE('',*,*,#16524,.F.);
#23542=ORIENTED_EDGE('',*,*,#16525,.T.);
#23543=ORIENTED_EDGE('',*,*,#16522,.T.);
#23544=ORIENTED_EDGE('',*,*,#16525,.F.);
#23545=ORIENTED_EDGE('',*,*,#16526,.F.);
#23546=ORIENTED_EDGE('',*,*,#16527,.T.);
#23547=ORIENTED_EDGE('',*,*,#16524,.T.);
#23548=ORIENTED_EDGE('',*,*,#16527,.F.);
#23549=ORIENTED_EDGE('',*,*,#16526,.T.);
#23550=CONICAL_SURFACE('',#25108,8.75,0.785398163397447);
#23551=CONICAL_SURFACE('',#25115,8.75,0.785398163397447);
#23552=CONICAL_SURFACE('',#25122,10.25,0.785398163397449);
#23553=CONICAL_SURFACE('',#25130,10.25,0.785398163397448);
#23554=CONICAL_SURFACE('',#25168,5.3,0.785398163397446);
#23555=CONICAL_SURFACE('',#25172,5.3,0.785398163397446);
#23556=CONICAL_SURFACE('',#25190,5.3,0.785398163397446);
#23557=CONICAL_SURFACE('',#25206,5.3,0.785398163397446);
#23558=CONICAL_SURFACE('',#25207,5.3,0.785398163397446);
#23559=CONICAL_SURFACE('',#25208,5.3,0.785398163397446);
#23560=CONICAL_SURFACE('',#25209,5.75,0.785398163397446);
#23561=CONICAL_SURFACE('',#25213,5.75,0.785398163397446);
#23562=CONICAL_SURFACE('',#25223,5.75,0.785398163397447);
#23563=CONICAL_SURFACE('',#25224,5.75,0.785398163397447);
#23564=CONICAL_SURFACE('',#25226,1.25,0.785398163397465);
#23565=CONICAL_SURFACE('',#25230,1.25,0.785398163397454);
#23566=CONICAL_SURFACE('',#25446,13.8,0.785398163397448);
#23567=CONICAL_SURFACE('',#25453,13.8,0.785398163397448);
#23568=CONICAL_SURFACE('',#25563,7.45,0.785398163397442);
#23569=CONICAL_SURFACE('',#25571,24.8,0.785398163397439);
#23570=CONICAL_SURFACE('',#25575,24.8,0.785398163397439);
#23571=CONICAL_SURFACE('',#25593,22.2,0.785398163397439);
#23572=CONICAL_SURFACE('',#25597,22.2,0.785398163397439);
#23573=CONICAL_SURFACE('',#25604,8.75,0.785398163397439);
#23574=CONICAL_SURFACE('',#25610,8.75,0.785398163397439);
#23575=CONICAL_SURFACE('',#25615,8.75,0.785398163397439);
#23576=CONICAL_SURFACE('',#25622,8.75,0.785398163397439);
#23577=CONICAL_SURFACE('',#25628,9.74999999999999,0.785398163397441);
#23578=CONICAL_SURFACE('',#25631,9.75,0.785398163397441);
#23579=CONICAL_SURFACE('',#25634,9.74999999999999,0.785398163397441);
#23580=CONICAL_SURFACE('',#25637,9.74999999999999,0.785398163397441);
#23581=CONICAL_SURFACE('',#25647,9.82322330470336,0.392699081698712);
#23582=CONICAL_SURFACE('',#25650,9.82322330470335,0.392699081698721);
#23583=CONICAL_SURFACE('',#25653,9.82322330470336,0.392699081698712);
#23584=CONICAL_SURFACE('',#25657,9.82322330470335,0.392699081698725);
#23585=CONICAL_SURFACE('',#25660,9.25,0.785398163397447);
#23586=CONICAL_SURFACE('',#25663,9.24999999999999,0.785398163397447);
#23587=CONICAL_SURFACE('',#25665,9.24999999999999,0.785398163397446);
#23588=CONICAL_SURFACE('',#25668,9.24999999999999,0.785398163397446);
#23589=CONICAL_SURFACE('',#26055,7.69,0.785398163397446);
#23590=CONICAL_SURFACE('',#26436,9.47407799863807,1.24294851367413);
#23591=CONICAL_SURFACE('',#26442,10.15,0.915100700553361);
#23592=CONICAL_SURFACE('',#26456,9.07,0.846355413487022);
#23593=CONICAL_SURFACE('',#26460,12.3,0.785398163397449);
#23594=CONICAL_SURFACE('',#26471,12.3,0.785398163397449);
#23595=CONICAL_SURFACE('',#26481,0.900000000000001,0.785398163397449);
#23596=CONICAL_SURFACE('',#26485,0.900000000000001,0.785398163397449);
#23597=CONICAL_SURFACE('',#26489,0.900000000000001,0.785398163397449);
#23598=CONICAL_SURFACE('',#26493,0.900000000000001,0.785398163397449);
#23599=CONICAL_SURFACE('',#26567,9.4,1.04718484902493);
#23600=CONICAL_SURFACE('',#26573,6.89,0.785398163397448);
#23601=CONICAL_SURFACE('',#26884,4.75,0.785398163397441);
#23602=CONICAL_SURFACE('',#26887,4.975,0.0996686524911625);
#23603=CONICAL_SURFACE('',#26895,7.75,0.785398163397448);
#23604=CONICAL_SURFACE('',#26901,3.8,0.785398163397449);
#23605=CONICAL_SURFACE('',#26905,3.8,0.785398163397448);
#23606=ADVANCED_FACE('',(#1747),#23550,.T.);
#23607=ADVANCED_FACE('',(#1748,#586),#711,.F.);
#23608=ADVANCED_FACE('',(#1749),#400,.T.);
#23609=ADVANCED_FACE('',(#1750),#23551,.T.);
#23610=ADVANCED_FACE('',(#1751,#587),#712,.F.);
#23611=ADVANCED_FACE('',(#1752),#401,.T.);
#23612=ADVANCED_FACE('',(#1753),#23552,.F.);
#23613=ADVANCED_FACE('',(#1754),#402,.F.);
#23614=ADVANCED_FACE('',(#1755,#588),#713,.F.);
#23615=ADVANCED_FACE('',(#1756),#23553,.F.);
#23616=ADVANCED_FACE('',(#1757,#589),#714,.T.);
#23617=ADVANCED_FACE('',(#1758),#390,.T.);
#23618=ADVANCED_FACE('',(#1759),#391,.T.);
#23619=ADVANCED_FACE('',(#1760),#715,.T.);
#23620=ADVANCED_FACE('',(#1761,#590,#591,#592,#593,#594,#595),#716,.F.);
#23621=ADVANCED_FACE('',(#1762),#403,.T.);
#23622=ADVANCED_FACE('',(#1763),#717,.T.);
#23623=ADVANCED_FACE('',(#1764),#392,.T.);
#23624=ADVANCED_FACE('',(#1765),#393,.T.);
#23625=ADVANCED_FACE('',(#1766),#718,.T.);
#23626=ADVANCED_FACE('',(#1767),#404,.T.);
#23627=ADVANCED_FACE('',(#1768),#719,.T.);
#23628=ADVANCED_FACE('',(#1769),#23554,.F.);
#23629=ADVANCED_FACE('',(#1770),#405,.F.);
#23630=ADVANCED_FACE('',(#1771),#23555,.F.);
#23631=ADVANCED_FACE('',(#1772),#406,.F.);
#23632=ADVANCED_FACE('',(#1773),#720,.T.);
#23633=ADVANCED_FACE('',(#1774),#407,.F.);
#23634=ADVANCED_FACE('',(#1775),#721,.T.);
#23635=ADVANCED_FACE('',(#1776),#408,.F.);
#23636=ADVANCED_FACE('',(#1777),#722,.T.);
#23637=ADVANCED_FACE('',(#1778),#723,.T.);
#23638=ADVANCED_FACE('',(#1779),#23556,.F.);
#23639=ADVANCED_FACE('',(#1780,#596,#597,#598,#599,#600,#601,#602,#603,
#604),#724,.T.);
#23640=ADVANCED_FACE('',(#1781),#23557,.F.);
#23641=ADVANCED_FACE('',(#1782),#23558,.F.);
#23642=ADVANCED_FACE('',(#1783),#23559,.F.);
#23643=ADVANCED_FACE('',(#1784),#23560,.F.);
#23644=ADVANCED_FACE('',(#1785),#409,.F.);
#23645=ADVANCED_FACE('',(#1786),#23561,.F.);
#23646=ADVANCED_FACE('',(#1787),#410,.F.);
#23647=ADVANCED_FACE('',(#1788),#394,.T.);
#23648=ADVANCED_FACE('',(#1789),#395,.T.);
#23649=ADVANCED_FACE('',(#1790),#725,.T.);
#23650=ADVANCED_FACE('',(#1791),#411,.T.);
#23651=ADVANCED_FACE('',(#1792),#726,.T.);
#23652=ADVANCED_FACE('',(#1793),#396,.T.);
#23653=ADVANCED_FACE('',(#1794),#397,.T.);
#23654=ADVANCED_FACE('',(#1795),#727,.T.);
#23655=ADVANCED_FACE('',(#1796),#412,.T.);
#23656=ADVANCED_FACE('',(#1797),#728,.T.);
#23657=ADVANCED_FACE('',(#1798),#23562,.F.);
#23658=ADVANCED_FACE('',(#1799),#23563,.F.);
#23659=ADVANCED_FACE('',(#1800),#729,.T.);
#23660=ADVANCED_FACE('',(#1801),#23564,.T.);
#23661=ADVANCED_FACE('',(#1802),#730,.T.);
#23662=ADVANCED_FACE('',(#1803),#23565,.T.);
#23663=ADVANCED_FACE('',(#1804),#731,.T.);
#23664=ADVANCED_FACE('',(#1805),#732,.T.);
#23665=ADVANCED_FACE('',(#1806),#192,.T.);
#23666=ADVANCED_FACE('',(#1807),#413,.T.);
#23667=ADVANCED_FACE('',(#1808),#193,.T.);
#23668=ADVANCED_FACE('',(#1809),#194,.T.);
#23669=ADVANCED_FACE('',(#1810),#195,.T.);
#23670=ADVANCED_FACE('',(#1811),#414,.T.);
#23671=ADVANCED_FACE('',(#1812),#415,.T.);
#23672=ADVANCED_FACE('',(#1813),#416,.T.);
#23673=ADVANCED_FACE('',(#1814),#733,.F.);
#23674=ADVANCED_FACE('',(#1815),#417,.F.);
#23675=ADVANCED_FACE('',(#1816),#196,.T.);
#23676=ADVANCED_FACE('',(#1817),#197,.T.);
#23677=ADVANCED_FACE('',(#1818),#198,.T.);
#23678=ADVANCED_FACE('',(#1819),#418,.T.);
#23679=ADVANCED_FACE('',(#1820),#419,.T.);
#23680=ADVANCED_FACE('',(#1821),#420,.T.);
#23681=ADVANCED_FACE('',(#1822),#734,.F.);
#23682=ADVANCED_FACE('',(#1823),#421,.F.);
#23683=ADVANCED_FACE('',(#1824),#199,.T.);
#23684=ADVANCED_FACE('',(#1825),#200,.T.);
#23685=ADVANCED_FACE('',(#1826),#422,.T.);
#23686=ADVANCED_FACE('',(#1827),#201,.T.);
#23687=ADVANCED_FACE('',(#1828),#423,.T.);
#23688=ADVANCED_FACE('',(#1829),#424,.T.);
#23689=ADVANCED_FACE('',(#1830),#202,.T.);
#23690=ADVANCED_FACE('',(#1831),#203,.T.);
#23691=ADVANCED_FACE('',(#1832),#204,.T.);
#23692=ADVANCED_FACE('',(#1833),#425,.T.);
#23693=ADVANCED_FACE('',(#1834),#205,.T.);
#23694=ADVANCED_FACE('',(#1835),#426,.T.);
#23695=ADVANCED_FACE('',(#1836),#735,.F.);
#23696=ADVANCED_FACE('',(#1837),#427,.F.);
#23697=ADVANCED_FACE('',(#1838),#736,.F.);
#23698=ADVANCED_FACE('',(#1839),#428,.F.);
#23699=ADVANCED_FACE('',(#1840),#737,.F.);
#23700=ADVANCED_FACE('',(#1841),#429,.T.);
#23701=ADVANCED_FACE('',(#1842),#430,.T.);
#23702=ADVANCED_FACE('',(#1843),#431,.T.);
#23703=ADVANCED_FACE('',(#1844),#206,.T.);
#23704=ADVANCED_FACE('',(#1845),#432,.T.);
#23705=ADVANCED_FACE('',(#1846),#207,.T.);
#23706=ADVANCED_FACE('',(#1847),#433,.T.);
#23707=ADVANCED_FACE('',(#1848),#208,.T.);
#23708=ADVANCED_FACE('',(#1849),#434,.T.);
#23709=ADVANCED_FACE('',(#1850),#209,.T.);
#23710=ADVANCED_FACE('',(#1851),#435,.T.);
#23711=ADVANCED_FACE('',(#1852),#436,.T.);
#23712=ADVANCED_FACE('',(#1853),#738,.T.);
#23713=ADVANCED_FACE('',(#1854),#437,.T.);
#23714=ADVANCED_FACE('',(#1855),#739,.T.);
#23715=ADVANCED_FACE('',(#1856),#438,.T.);
#23716=ADVANCED_FACE('',(#1857),#439,.T.);
#23717=ADVANCED_FACE('',(#1858),#740,.T.);
#23718=ADVANCED_FACE('',(#1859),#440,.T.);
#23719=ADVANCED_FACE('',(#1860),#741,.T.);
#23720=ADVANCED_FACE('',(#1861),#210,.T.);
#23721=ADVANCED_FACE('',(#1862),#441,.T.);
#23722=ADVANCED_FACE('',(#1863),#211,.T.);
#23723=ADVANCED_FACE('',(#1864),#442,.T.);
#23724=ADVANCED_FACE('',(#1865),#742,.T.);
#23725=ADVANCED_FACE('',(#1866),#443,.T.);
#23726=ADVANCED_FACE('',(#1867),#212,.T.);
#23727=ADVANCED_FACE('',(#1868),#444,.T.);
#23728=ADVANCED_FACE('',(#1869),#213,.T.);
#23729=ADVANCED_FACE('',(#1870),#445,.T.);
#23730=ADVANCED_FACE('',(#1871),#214,.T.);
#23731=ADVANCED_FACE('',(#1872),#446,.T.);
#23732=ADVANCED_FACE('',(#1873),#215,.T.);
#23733=ADVANCED_FACE('',(#1874),#447,.T.);
#23734=ADVANCED_FACE('',(#1875),#216,.T.);
#23735=ADVANCED_FACE('',(#1876),#448,.T.);
#23736=ADVANCED_FACE('',(#1877,#605),#743,.T.);
#23737=ADVANCED_FACE('',(#1878),#449,.T.);
#23738=ADVANCED_FACE('',(#1879),#744,.T.);
#23739=ADVANCED_FACE('',(#1880),#217,.T.);
#23740=ADVANCED_FACE('',(#1881),#218,.T.);
#23741=ADVANCED_FACE('',(#1882),#745,.T.);
#23742=ADVANCED_FACE('',(#1883),#219,.T.);
#23743=ADVANCED_FACE('',(#1884),#220,.T.);
#23744=ADVANCED_FACE('',(#1885),#746,.T.);
#23745=ADVANCED_FACE('',(#1886),#450,.T.);
#23746=ADVANCED_FACE('',(#1887),#221,.T.);
#23747=ADVANCED_FACE('',(#1888),#451,.T.);
#23748=ADVANCED_FACE('',(#1889),#222,.T.);
#23749=ADVANCED_FACE('',(#1890),#452,.F.);
#23750=ADVANCED_FACE('',(#1891),#747,.F.);
#23751=ADVANCED_FACE('',(#1892),#453,.T.);
#23752=ADVANCED_FACE('',(#1893),#223,.T.);
#23753=ADVANCED_FACE('',(#1894),#454,.T.);
#23754=ADVANCED_FACE('',(#1895),#224,.T.);
#23755=ADVANCED_FACE('',(#1896),#455,.T.);
#23756=ADVANCED_FACE('',(#1897),#748,.F.);
#23757=ADVANCED_FACE('',(#1898),#456,.T.);
#23758=ADVANCED_FACE('',(#1899),#749,.F.);
#23759=ADVANCED_FACE('',(#1900),#457,.F.);
#23760=ADVANCED_FACE('',(#1901),#750,.F.);
#23761=ADVANCED_FACE('',(#1902,#606),#751,.T.);
#23762=ADVANCED_FACE('',(#1903),#458,.F.);
#23763=ADVANCED_FACE('',(#1904),#752,.T.);
#23764=ADVANCED_FACE('',(#1905),#459,.F.);
#23765=ADVANCED_FACE('',(#1906),#753,.T.);
#23766=ADVANCED_FACE('',(#1907,#607),#754,.F.);
#23767=ADVANCED_FACE('',(#1908),#460,.F.);
#23768=ADVANCED_FACE('',(#1909,#608),#755,.F.);
#23769=ADVANCED_FACE('',(#1910),#461,.F.);
#23770=ADVANCED_FACE('',(#1911),#462,.F.);
#23771=ADVANCED_FACE('',(#1912,#609,#610),#756,.F.);
#23772=ADVANCED_FACE('',(#1913),#463,.T.);
#23773=ADVANCED_FACE('',(#1914),#464,.T.);
#23774=ADVANCED_FACE('',(#1915),#757,.T.);
#23775=ADVANCED_FACE('',(#1916),#758,.T.);
#23776=ADVANCED_FACE('',(#1917),#759,.F.);
#23777=ADVANCED_FACE('',(#1918),#760,.F.);
#23778=ADVANCED_FACE('',(#1919),#761,.F.);
#23779=ADVANCED_FACE('',(#1920),#762,.F.);
#23780=ADVANCED_FACE('',(#1921),#763,.T.);
#23781=ADVANCED_FACE('',(#1922),#465,.T.);
#23782=ADVANCED_FACE('',(#1923),#23566,.F.);
#23783=ADVANCED_FACE('',(#1924),#466,.F.);
#23784=ADVANCED_FACE('',(#1925,#611),#764,.T.);
#23785=ADVANCED_FACE('',(#1926),#23567,.F.);
#23786=ADVANCED_FACE('',(#1927),#467,.F.);
#23787=ADVANCED_FACE('',(#1928,#612),#765,.F.);
#23788=ADVANCED_FACE('',(#1929),#468,.T.);
#23789=ADVANCED_FACE('',(#1930),#225,.T.);
#23790=ADVANCED_FACE('',(#1931),#469,.T.);
#23791=ADVANCED_FACE('',(#1932),#226,.T.);
#23792=ADVANCED_FACE('',(#1933),#470,.T.);
#23793=ADVANCED_FACE('',(#1934),#227,.T.);
#23794=ADVANCED_FACE('',(#1935),#471,.T.);
#23795=ADVANCED_FACE('',(#1936),#228,.T.);
#23796=ADVANCED_FACE('',(#1937),#472,.T.);
#23797=ADVANCED_FACE('',(#1938),#766,.T.);
#23798=ADVANCED_FACE('',(#1939),#473,.T.);
#23799=ADVANCED_FACE('',(#1940,#613),#767,.T.);
#23800=ADVANCED_FACE('',(#1941,#614,#615,#616,#617,#618,#619,#620),#768,
 .T.);
#23801=ADVANCED_FACE('',(#1942),#474,.T.);
#23802=ADVANCED_FACE('',(#1943),#229,.T.);
#23803=ADVANCED_FACE('',(#1944),#475,.T.);
#23804=ADVANCED_FACE('',(#1945),#230,.T.);
#23805=ADVANCED_FACE('',(#1946),#476,.T.);
#23806=ADVANCED_FACE('',(#1947),#231,.T.);
#23807=ADVANCED_FACE('',(#1948),#477,.T.);
#23808=ADVANCED_FACE('',(#1949),#232,.T.);
#23809=ADVANCED_FACE('',(#1950),#478,.T.);
#23810=ADVANCED_FACE('',(#1951),#769,.T.);
#23811=ADVANCED_FACE('',(#1952),#479,.T.);
#23812=ADVANCED_FACE('',(#1953,#621,#622,#623,#624,#625,#626,#627),#770,
 .F.);
#23813=ADVANCED_FACE('',(#1954),#480,.F.);
#23814=ADVANCED_FACE('',(#1955),#771,.T.);
#23815=ADVANCED_FACE('',(#1956),#481,.F.);
#23816=ADVANCED_FACE('',(#1957),#772,.T.);
#23817=ADVANCED_FACE('',(#1958),#482,.F.);
#23818=ADVANCED_FACE('',(#1959),#773,.F.);
#23819=ADVANCED_FACE('',(#1960),#483,.F.);
#23820=ADVANCED_FACE('',(#1961),#774,.F.);
#23821=ADVANCED_FACE('',(#1962),#484,.F.);
#23822=ADVANCED_FACE('',(#1963),#485,.F.);
#23823=ADVANCED_FACE('',(#1964),#486,.F.);
#23824=ADVANCED_FACE('',(#1965),#487,.F.);
#23825=ADVANCED_FACE('',(#1966),#488,.F.);
#23826=ADVANCED_FACE('',(#1967),#489,.F.);
#23827=ADVANCED_FACE('',(#1968,#628),#775,.F.);
#23828=ADVANCED_FACE('',(#1969),#490,.F.);
#23829=ADVANCED_FACE('',(#1970),#491,.F.);
#23830=ADVANCED_FACE('',(#1971),#492,.F.);
#23831=ADVANCED_FACE('',(#1972,#629),#776,.T.);
#23832=ADVANCED_FACE('',(#1973),#493,.F.);
#23833=ADVANCED_FACE('',(#1974,#630),#777,.T.);
#23834=ADVANCED_FACE('',(#1975),#23568,.F.);
#23835=ADVANCED_FACE('',(#1976,#631),#778,.T.);
#23836=ADVANCED_FACE('',(#1977),#494,.F.);
#23837=ADVANCED_FACE('',(#1978),#779,.T.);
#23838=ADVANCED_FACE('',(#1979),#23569,.F.);
#23839=ADVANCED_FACE('',(#1980),#780,.T.);
#23840=ADVANCED_FACE('',(#1981),#23570,.F.);
#23841=ADVANCED_FACE('',(#1982),#495,.F.);
#23842=ADVANCED_FACE('',(#1983),#781,.F.);
#23843=ADVANCED_FACE('',(#1984,#632,#633,#634,#635,#636,#637,#638),#782,
 .F.);
#23844=ADVANCED_FACE('',(#1985),#783,.T.);
#23845=ADVANCED_FACE('',(#1986),#23571,.T.);
#23846=ADVANCED_FACE('',(#1987),#784,.T.);
#23847=ADVANCED_FACE('',(#1988),#23572,.T.);
#23848=ADVANCED_FACE('',(#1989),#496,.T.);
#23849=ADVANCED_FACE('',(#1990),#785,.F.);
#23850=ADVANCED_FACE('',(#1991),#786,.F.);
#23851=ADVANCED_FACE('',(#1992),#23573,.F.);
#23852=ADVANCED_FACE('',(#1993),#787,.T.);
#23853=ADVANCED_FACE('',(#1994),#497,.F.);
#23854=ADVANCED_FACE('',(#1995),#23574,.F.);
#23855=ADVANCED_FACE('',(#1996),#498,.F.);
#23856=ADVANCED_FACE('',(#1997),#23575,.F.);
#23857=ADVANCED_FACE('',(#1998),#788,.T.);
#23858=ADVANCED_FACE('',(#1999),#499,.F.);
#23859=ADVANCED_FACE('',(#2000),#23576,.F.);
#23860=ADVANCED_FACE('',(#2001),#500,.F.);
#23861=ADVANCED_FACE('',(#2002),#23577,.T.);
#23862=ADVANCED_FACE('',(#2003),#789,.T.);
#23863=ADVANCED_FACE('',(#2004),#23578,.T.);
#23864=ADVANCED_FACE('',(#2005),#790,.T.);
#23865=ADVANCED_FACE('',(#2006),#23579,.T.);
#23866=ADVANCED_FACE('',(#2007),#791,.T.);
#23867=ADVANCED_FACE('',(#2008),#23580,.T.);
#23868=ADVANCED_FACE('',(#2009),#792,.T.);
#23869=ADVANCED_FACE('',(#2010),#793,.T.);
#23870=ADVANCED_FACE('',(#2011),#501,.T.);
#23871=ADVANCED_FACE('',(#2012),#794,.T.);
#23872=ADVANCED_FACE('',(#2013),#502,.T.);
#23873=ADVANCED_FACE('',(#2014),#795,.T.);
#23874=ADVANCED_FACE('',(#2015),#23581,.T.);
#23875=ADVANCED_FACE('',(#2016),#796,.T.);
#23876=ADVANCED_FACE('',(#2017),#23582,.T.);
#23877=ADVANCED_FACE('',(#2018),#797,.T.);
#23878=ADVANCED_FACE('',(#2019),#23583,.T.);
#23879=ADVANCED_FACE('',(#2020),#798,.T.);
#23880=ADVANCED_FACE('',(#2021),#23584,.T.);
#23881=ADVANCED_FACE('',(#2022),#23585,.T.);
#23882=ADVANCED_FACE('',(#2023),#799,.T.);
#23883=ADVANCED_FACE('',(#2024),#23586,.T.);
#23884=ADVANCED_FACE('',(#2025),#23587,.T.);
#23885=ADVANCED_FACE('',(#2026),#800,.T.);
#23886=ADVANCED_FACE('',(#2027),#23588,.T.);
#23887=ADVANCED_FACE('',(#2028,#639),#801,.T.);
#23888=ADVANCED_FACE('',(#2029),#503,.T.);
#23889=ADVANCED_FACE('',(#2030),#802,.F.);
#23890=ADVANCED_FACE('',(#2031),#504,.F.);
#23891=ADVANCED_FACE('',(#2032),#803,.F.);
#23892=ADVANCED_FACE('',(#2033,#640),#804,.F.);
#23893=ADVANCED_FACE('',(#2034),#505,.F.);
#23894=ADVANCED_FACE('',(#2035),#805,.T.);
#23895=ADVANCED_FACE('',(#2036),#506,.F.);
#23896=ADVANCED_FACE('',(#2037),#806,.F.);
#23897=ADVANCED_FACE('',(#2038),#507,.F.);
#23898=ADVANCED_FACE('',(#2039),#807,.F.);
#23899=ADVANCED_FACE('',(#2040),#508,.F.);
#23900=ADVANCED_FACE('',(#2041),#509,.F.);
#23901=ADVANCED_FACE('',(#2042),#510,.F.);
#23902=ADVANCED_FACE('',(#2043),#511,.F.);
#23903=ADVANCED_FACE('',(#2044,#641),#808,.T.);
#23904=ADVANCED_FACE('',(#2045,#642),#809,.T.);
#23905=ADVANCED_FACE('',(#2046,#643),#810,.T.);
#23906=ADVANCED_FACE('',(#2047,#644),#811,.T.);
#23907=ADVANCED_FACE('',(#2048),#512,.T.);
#23908=ADVANCED_FACE('',(#2049),#812,.T.);
#23909=ADVANCED_FACE('',(#2050),#513,.T.);
#23910=ADVANCED_FACE('',(#2051),#813,.T.);
#23911=ADVANCED_FACE('',(#2052),#814,.T.);
#23912=ADVANCED_FACE('',(#2053,#645),#815,.F.);
#23913=ADVANCED_FACE('',(#2054),#816,.T.);
#23914=ADVANCED_FACE('',(#2055),#817,.T.);
#23915=ADVANCED_FACE('',(#2056),#818,.T.);
#23916=ADVANCED_FACE('',(#2057),#819,.T.);
#23917=ADVANCED_FACE('',(#2058),#820,.T.);
#23918=ADVANCED_FACE('',(#2059),#821,.T.);
#23919=ADVANCED_FACE('',(#2060),#822,.T.);
#23920=ADVANCED_FACE('',(#2061),#823,.T.);
#23921=ADVANCED_FACE('',(#2062),#824,.T.);
#23922=ADVANCED_FACE('',(#2063),#825,.T.);
#23923=ADVANCED_FACE('',(#2064),#826,.T.);
#23924=ADVANCED_FACE('',(#2065),#827,.T.);
#23925=ADVANCED_FACE('',(#2066),#828,.T.);
#23926=ADVANCED_FACE('',(#2067),#829,.T.);
#23927=ADVANCED_FACE('',(#2068),#830,.T.);
#23928=ADVANCED_FACE('',(#2069),#831,.T.);
#23929=ADVANCED_FACE('',(#2070),#832,.T.);
#23930=ADVANCED_FACE('',(#2071),#833,.T.);
#23931=ADVANCED_FACE('',(#2072),#834,.T.);
#23932=ADVANCED_FACE('',(#2073),#835,.T.);
#23933=ADVANCED_FACE('',(#2074),#836,.T.);
#23934=ADVANCED_FACE('',(#2075),#837,.T.);
#23935=ADVANCED_FACE('',(#2076),#838,.T.);
#23936=ADVANCED_FACE('',(#2077),#839,.T.);
#23937=ADVANCED_FACE('',(#2078),#840,.T.);
#23938=ADVANCED_FACE('',(#2079),#841,.T.);
#23939=ADVANCED_FACE('',(#2080),#842,.T.);
#23940=ADVANCED_FACE('',(#2081),#843,.T.);
#23941=ADVANCED_FACE('',(#2082),#844,.T.);
#23942=ADVANCED_FACE('',(#2083),#845,.T.);
#23943=ADVANCED_FACE('',(#2084),#846,.T.);
#23944=ADVANCED_FACE('',(#2085),#847,.T.);
#23945=ADVANCED_FACE('',(#2086),#848,.T.);
#23946=ADVANCED_FACE('',(#2087),#849,.T.);
#23947=ADVANCED_FACE('',(#2088),#850,.T.);
#23948=ADVANCED_FACE('',(#2089),#851,.T.);
#23949=ADVANCED_FACE('',(#2090),#852,.T.);
#23950=ADVANCED_FACE('',(#2091),#853,.T.);
#23951=ADVANCED_FACE('',(#2092),#854,.T.);
#23952=ADVANCED_FACE('',(#2093),#855,.T.);
#23953=ADVANCED_FACE('',(#2094),#856,.T.);
#23954=ADVANCED_FACE('',(#2095),#857,.T.);
#23955=ADVANCED_FACE('',(#2096),#858,.T.);
#23956=ADVANCED_FACE('',(#2097),#859,.T.);
#23957=ADVANCED_FACE('',(#2098),#860,.T.);
#23958=ADVANCED_FACE('',(#2099),#861,.T.);
#23959=ADVANCED_FACE('',(#2100),#862,.T.);
#23960=ADVANCED_FACE('',(#2101),#863,.T.);
#23961=ADVANCED_FACE('',(#2102),#864,.T.);
#23962=ADVANCED_FACE('',(#2103),#865,.T.);
#23963=ADVANCED_FACE('',(#2104),#866,.T.);
#23964=ADVANCED_FACE('',(#2105),#867,.T.);
#23965=ADVANCED_FACE('',(#2106),#868,.T.);
#23966=ADVANCED_FACE('',(#2107),#869,.T.);
#23967=ADVANCED_FACE('',(#2108),#870,.T.);
#23968=ADVANCED_FACE('',(#2109),#871,.T.);
#23969=ADVANCED_FACE('',(#2110),#872,.T.);
#23970=ADVANCED_FACE('',(#2111),#873,.T.);
#23971=ADVANCED_FACE('',(#2112),#874,.T.);
#23972=ADVANCED_FACE('',(#2113),#875,.T.);
#23973=ADVANCED_FACE('',(#2114),#876,.T.);
#23974=ADVANCED_FACE('',(#2115),#877,.T.);
#23975=ADVANCED_FACE('',(#2116),#878,.T.);
#23976=ADVANCED_FACE('',(#2117),#879,.T.);
#23977=ADVANCED_FACE('',(#2118),#880,.T.);
#23978=ADVANCED_FACE('',(#2119),#881,.T.);
#23979=ADVANCED_FACE('',(#2120),#882,.T.);
#23980=ADVANCED_FACE('',(#2121),#883,.T.);
#23981=ADVANCED_FACE('',(#2122),#884,.T.);
#23982=ADVANCED_FACE('',(#2123),#885,.T.);
#23983=ADVANCED_FACE('',(#2124),#886,.T.);
#23984=ADVANCED_FACE('',(#2125),#887,.T.);
#23985=ADVANCED_FACE('',(#2126,#646),#888,.T.);
#23986=ADVANCED_FACE('',(#2127),#889,.T.);
#23987=ADVANCED_FACE('',(#2128),#890,.T.);
#23988=ADVANCED_FACE('',(#2129),#891,.T.);
#23989=ADVANCED_FACE('',(#2130),#892,.T.);
#23990=ADVANCED_FACE('',(#2131),#893,.T.);
#23991=ADVANCED_FACE('',(#2132),#894,.T.);
#23992=ADVANCED_FACE('',(#2133),#895,.T.);
#23993=ADVANCED_FACE('',(#2134),#896,.T.);
#23994=ADVANCED_FACE('',(#2135),#897,.T.);
#23995=ADVANCED_FACE('',(#2136),#898,.T.);
#23996=ADVANCED_FACE('',(#2137),#899,.T.);
#23997=ADVANCED_FACE('',(#2138),#900,.T.);
#23998=ADVANCED_FACE('',(#2139),#901,.T.);
#23999=ADVANCED_FACE('',(#2140),#902,.T.);
#24000=ADVANCED_FACE('',(#2141),#903,.T.);
#24001=ADVANCED_FACE('',(#2142),#904,.T.);
#24002=ADVANCED_FACE('',(#2143),#905,.T.);
#24003=ADVANCED_FACE('',(#2144),#906,.T.);
#24004=ADVANCED_FACE('',(#2145),#907,.T.);
#24005=ADVANCED_FACE('',(#2146),#908,.T.);
#24006=ADVANCED_FACE('',(#2147),#909,.T.);
#24007=ADVANCED_FACE('',(#2148),#910,.T.);
#24008=ADVANCED_FACE('',(#2149),#911,.T.);
#24009=ADVANCED_FACE('',(#2150),#912,.F.);
#24010=ADVANCED_FACE('',(#2151),#913,.F.);
#24011=ADVANCED_FACE('',(#2152),#914,.F.);
#24012=ADVANCED_FACE('',(#2153),#915,.F.);
#24013=ADVANCED_FACE('',(#2154),#916,.F.);
#24014=ADVANCED_FACE('',(#2155),#917,.T.);
#24015=ADVANCED_FACE('',(#2156),#918,.T.);
#24016=ADVANCED_FACE('',(#2157),#919,.T.);
#24017=ADVANCED_FACE('',(#2158),#920,.T.);
#24018=ADVANCED_FACE('',(#2159),#921,.T.);
#24019=ADVANCED_FACE('',(#2160),#922,.T.);
#24020=ADVANCED_FACE('',(#2161),#923,.T.);
#24021=ADVANCED_FACE('',(#2162),#924,.T.);
#24022=ADVANCED_FACE('',(#2163),#925,.T.);
#24023=ADVANCED_FACE('',(#2164),#926,.T.);
#24024=ADVANCED_FACE('',(#2165),#927,.T.);
#24025=ADVANCED_FACE('',(#2166),#928,.T.);
#24026=ADVANCED_FACE('',(#2167),#929,.T.);
#24027=ADVANCED_FACE('',(#2168),#930,.T.);
#24028=ADVANCED_FACE('',(#2169),#931,.T.);
#24029=ADVANCED_FACE('',(#2170),#932,.T.);
#24030=ADVANCED_FACE('',(#2171),#933,.T.);
#24031=ADVANCED_FACE('',(#2172),#934,.T.);
#24032=ADVANCED_FACE('',(#2173),#935,.T.);
#24033=ADVANCED_FACE('',(#2174),#936,.T.);
#24034=ADVANCED_FACE('',(#2175),#937,.T.);
#24035=ADVANCED_FACE('',(#2176),#938,.T.);
#24036=ADVANCED_FACE('',(#2177),#939,.T.);
#24037=ADVANCED_FACE('',(#2178),#940,.T.);
#24038=ADVANCED_FACE('',(#2179),#941,.T.);
#24039=ADVANCED_FACE('',(#2180),#942,.T.);
#24040=ADVANCED_FACE('',(#2181),#943,.T.);
#24041=ADVANCED_FACE('',(#2182),#944,.T.);
#24042=ADVANCED_FACE('',(#2183),#945,.T.);
#24043=ADVANCED_FACE('',(#2184),#946,.T.);
#24044=ADVANCED_FACE('',(#2185),#947,.T.);
#24045=ADVANCED_FACE('',(#2186),#948,.T.);
#24046=ADVANCED_FACE('',(#2187),#949,.T.);
#24047=ADVANCED_FACE('',(#2188),#950,.T.);
#24048=ADVANCED_FACE('',(#2189),#951,.T.);
#24049=ADVANCED_FACE('',(#2190),#952,.T.);
#24050=ADVANCED_FACE('',(#2191),#953,.T.);
#24051=ADVANCED_FACE('',(#2192),#954,.T.);
#24052=ADVANCED_FACE('',(#2193),#955,.T.);
#24053=ADVANCED_FACE('',(#2194),#956,.T.);
#24054=ADVANCED_FACE('',(#2195),#957,.T.);
#24055=ADVANCED_FACE('',(#2196),#958,.T.);
#24056=ADVANCED_FACE('',(#2197),#959,.T.);
#24057=ADVANCED_FACE('',(#2198),#960,.T.);
#24058=ADVANCED_FACE('',(#2199),#961,.T.);
#24059=ADVANCED_FACE('',(#2200),#962,.T.);
#24060=ADVANCED_FACE('',(#2201),#963,.T.);
#24061=ADVANCED_FACE('',(#2202),#964,.T.);
#24062=ADVANCED_FACE('',(#2203),#965,.T.);
#24063=ADVANCED_FACE('',(#2204),#966,.T.);
#24064=ADVANCED_FACE('',(#2205),#967,.T.);
#24065=ADVANCED_FACE('',(#2206),#968,.T.);
#24066=ADVANCED_FACE('',(#2207),#969,.T.);
#24067=ADVANCED_FACE('',(#2208),#970,.T.);
#24068=ADVANCED_FACE('',(#2209),#971,.T.);
#24069=ADVANCED_FACE('',(#2210),#972,.T.);
#24070=ADVANCED_FACE('',(#2211),#973,.T.);
#24071=ADVANCED_FACE('',(#2212),#974,.T.);
#24072=ADVANCED_FACE('',(#2213),#975,.T.);
#24073=ADVANCED_FACE('',(#2214),#976,.T.);
#24074=ADVANCED_FACE('',(#2215),#977,.T.);
#24075=ADVANCED_FACE('',(#2216),#978,.T.);
#24076=ADVANCED_FACE('',(#2217),#979,.T.);
#24077=ADVANCED_FACE('',(#2218),#980,.T.);
#24078=ADVANCED_FACE('',(#2219),#981,.T.);
#24079=ADVANCED_FACE('',(#2220),#982,.T.);
#24080=ADVANCED_FACE('',(#2221),#983,.T.);
#24081=ADVANCED_FACE('',(#2222),#984,.T.);
#24082=ADVANCED_FACE('',(#2223),#985,.T.);
#24083=ADVANCED_FACE('',(#2224),#986,.T.);
#24084=ADVANCED_FACE('',(#2225),#987,.T.);
#24085=ADVANCED_FACE('',(#2226),#988,.T.);
#24086=ADVANCED_FACE('',(#2227),#989,.T.);
#24087=ADVANCED_FACE('',(#2228),#990,.T.);
#24088=ADVANCED_FACE('',(#2229),#991,.T.);
#24089=ADVANCED_FACE('',(#2230),#992,.T.);
#24090=ADVANCED_FACE('',(#2231),#993,.T.);
#24091=ADVANCED_FACE('',(#2232),#994,.T.);
#24092=ADVANCED_FACE('',(#2233),#995,.T.);
#24093=ADVANCED_FACE('',(#2234),#996,.T.);
#24094=ADVANCED_FACE('',(#2235),#997,.T.);
#24095=ADVANCED_FACE('',(#2236),#998,.T.);
#24096=ADVANCED_FACE('',(#2237),#999,.T.);
#24097=ADVANCED_FACE('',(#2238),#1000,.T.);
#24098=ADVANCED_FACE('',(#2239),#1001,.T.);
#24099=ADVANCED_FACE('',(#2240),#1002,.T.);
#24100=ADVANCED_FACE('',(#2241),#1003,.T.);
#24101=ADVANCED_FACE('',(#2242),#1004,.T.);
#24102=ADVANCED_FACE('',(#2243),#1005,.T.);
#24103=ADVANCED_FACE('',(#2244),#1006,.T.);
#24104=ADVANCED_FACE('',(#2245),#1007,.T.);
#24105=ADVANCED_FACE('',(#2246),#1008,.T.);
#24106=ADVANCED_FACE('',(#2247),#1009,.T.);
#24107=ADVANCED_FACE('',(#2248),#1010,.T.);
#24108=ADVANCED_FACE('',(#2249),#1011,.T.);
#24109=ADVANCED_FACE('',(#2250),#1012,.T.);
#24110=ADVANCED_FACE('',(#2251),#1013,.T.);
#24111=ADVANCED_FACE('',(#2252),#1014,.T.);
#24112=ADVANCED_FACE('',(#2253),#1015,.T.);
#24113=ADVANCED_FACE('',(#2254),#1016,.T.);
#24114=ADVANCED_FACE('',(#2255),#1017,.T.);
#24115=ADVANCED_FACE('',(#2256),#1018,.T.);
#24116=ADVANCED_FACE('',(#2257),#1019,.T.);
#24117=ADVANCED_FACE('',(#2258),#1020,.T.);
#24118=ADVANCED_FACE('',(#2259),#1021,.T.);
#24119=ADVANCED_FACE('',(#2260),#1022,.T.);
#24120=ADVANCED_FACE('',(#2261),#1023,.T.);
#24121=ADVANCED_FACE('',(#2262),#1024,.T.);
#24122=ADVANCED_FACE('',(#2263),#1025,.T.);
#24123=ADVANCED_FACE('',(#2264),#1026,.T.);
#24124=ADVANCED_FACE('',(#2265),#1027,.T.);
#24125=ADVANCED_FACE('',(#2266),#1028,.T.);
#24126=ADVANCED_FACE('',(#2267),#1029,.T.);
#24127=ADVANCED_FACE('',(#2268),#1030,.T.);
#24128=ADVANCED_FACE('',(#2269),#1031,.T.);
#24129=ADVANCED_FACE('',(#2270),#1032,.T.);
#24130=ADVANCED_FACE('',(#2271),#1033,.T.);
#24131=ADVANCED_FACE('',(#2272),#1034,.T.);
#24132=ADVANCED_FACE('',(#2273),#1035,.T.);
#24133=ADVANCED_FACE('',(#2274),#1036,.T.);
#24134=ADVANCED_FACE('',(#2275),#1037,.T.);
#24135=ADVANCED_FACE('',(#2276),#1038,.T.);
#24136=ADVANCED_FACE('',(#2277),#1039,.T.);
#24137=ADVANCED_FACE('',(#2278),#1040,.T.);
#24138=ADVANCED_FACE('',(#2279),#1041,.T.);
#24139=ADVANCED_FACE('',(#2280),#1042,.T.);
#24140=ADVANCED_FACE('',(#2281),#1043,.T.);
#24141=ADVANCED_FACE('',(#2282),#1044,.T.);
#24142=ADVANCED_FACE('',(#2283),#1045,.T.);
#24143=ADVANCED_FACE('',(#2284),#1046,.T.);
#24144=ADVANCED_FACE('',(#2285),#1047,.T.);
#24145=ADVANCED_FACE('',(#2286),#1048,.T.);
#24146=ADVANCED_FACE('',(#2287),#1049,.T.);
#24147=ADVANCED_FACE('',(#2288),#1050,.T.);
#24148=ADVANCED_FACE('',(#2289),#1051,.T.);
#24149=ADVANCED_FACE('',(#2290),#1052,.T.);
#24150=ADVANCED_FACE('',(#2291),#1053,.T.);
#24151=ADVANCED_FACE('',(#2292),#1054,.T.);
#24152=ADVANCED_FACE('',(#2293),#1055,.T.);
#24153=ADVANCED_FACE('',(#2294),#1056,.T.);
#24154=ADVANCED_FACE('',(#2295),#1057,.T.);
#24155=ADVANCED_FACE('',(#2296),#1058,.T.);
#24156=ADVANCED_FACE('',(#2297),#1059,.T.);
#24157=ADVANCED_FACE('',(#2298),#1060,.T.);
#24158=ADVANCED_FACE('',(#2299),#1061,.T.);
#24159=ADVANCED_FACE('',(#2300),#1062,.T.);
#24160=ADVANCED_FACE('',(#2301),#1063,.T.);
#24161=ADVANCED_FACE('',(#2302),#1064,.T.);
#24162=ADVANCED_FACE('',(#2303),#1065,.T.);
#24163=ADVANCED_FACE('',(#2304),#1066,.T.);
#24164=ADVANCED_FACE('',(#2305),#1067,.T.);
#24165=ADVANCED_FACE('',(#2306),#1068,.T.);
#24166=ADVANCED_FACE('',(#2307),#1069,.T.);
#24167=ADVANCED_FACE('',(#2308),#1070,.T.);
#24168=ADVANCED_FACE('',(#2309),#1071,.T.);
#24169=ADVANCED_FACE('',(#2310),#1072,.T.);
#24170=ADVANCED_FACE('',(#2311),#1073,.T.);
#24171=ADVANCED_FACE('',(#2312),#1074,.T.);
#24172=ADVANCED_FACE('',(#2313),#1075,.T.);
#24173=ADVANCED_FACE('',(#2314),#1076,.T.);
#24174=ADVANCED_FACE('',(#2315),#1077,.T.);
#24175=ADVANCED_FACE('',(#2316),#1078,.T.);
#24176=ADVANCED_FACE('',(#2317),#1079,.T.);
#24177=ADVANCED_FACE('',(#2318),#1080,.T.);
#24178=ADVANCED_FACE('',(#2319),#1081,.T.);
#24179=ADVANCED_FACE('',(#2320),#1082,.T.);
#24180=ADVANCED_FACE('',(#2321),#1083,.T.);
#24181=ADVANCED_FACE('',(#2322),#1084,.T.);
#24182=ADVANCED_FACE('',(#2323),#1085,.T.);
#24183=ADVANCED_FACE('',(#2324),#1086,.T.);
#24184=ADVANCED_FACE('',(#2325),#1087,.T.);
#24185=ADVANCED_FACE('',(#2326),#1088,.T.);
#24186=ADVANCED_FACE('',(#2327),#1089,.T.);
#24187=ADVANCED_FACE('',(#2328),#1090,.T.);
#24188=ADVANCED_FACE('',(#2329),#1091,.T.);
#24189=ADVANCED_FACE('',(#2330),#1092,.T.);
#24190=ADVANCED_FACE('',(#2331),#1093,.T.);
#24191=ADVANCED_FACE('',(#2332),#1094,.T.);
#24192=ADVANCED_FACE('',(#2333),#1095,.T.);
#24193=ADVANCED_FACE('',(#2334),#1096,.T.);
#24194=ADVANCED_FACE('',(#2335),#1097,.T.);
#24195=ADVANCED_FACE('',(#2336),#1098,.T.);
#24196=ADVANCED_FACE('',(#2337),#1099,.T.);
#24197=ADVANCED_FACE('',(#2338),#1100,.T.);
#24198=ADVANCED_FACE('',(#2339),#1101,.T.);
#24199=ADVANCED_FACE('',(#2340),#1102,.T.);
#24200=ADVANCED_FACE('',(#2341),#1103,.T.);
#24201=ADVANCED_FACE('',(#2342),#1104,.T.);
#24202=ADVANCED_FACE('',(#2343),#1105,.T.);
#24203=ADVANCED_FACE('',(#2344),#1106,.T.);
#24204=ADVANCED_FACE('',(#2345),#1107,.T.);
#24205=ADVANCED_FACE('',(#2346),#1108,.T.);
#24206=ADVANCED_FACE('',(#2347),#1109,.T.);
#24207=ADVANCED_FACE('',(#2348),#1110,.T.);
#24208=ADVANCED_FACE('',(#2349),#1111,.T.);
#24209=ADVANCED_FACE('',(#2350),#1112,.T.);
#24210=ADVANCED_FACE('',(#2351),#1113,.T.);
#24211=ADVANCED_FACE('',(#2352),#1114,.T.);
#24212=ADVANCED_FACE('',(#2353),#1115,.T.);
#24213=ADVANCED_FACE('',(#2354),#1116,.T.);
#24214=ADVANCED_FACE('',(#2355),#1117,.T.);
#24215=ADVANCED_FACE('',(#2356),#1118,.T.);
#24216=ADVANCED_FACE('',(#2357),#1119,.T.);
#24217=ADVANCED_FACE('',(#2358),#1120,.T.);
#24218=ADVANCED_FACE('',(#2359),#1121,.T.);
#24219=ADVANCED_FACE('',(#2360),#1122,.T.);
#24220=ADVANCED_FACE('',(#2361),#1123,.T.);
#24221=ADVANCED_FACE('',(#2362),#1124,.T.);
#24222=ADVANCED_FACE('',(#2363),#1125,.T.);
#24223=ADVANCED_FACE('',(#2364),#1126,.T.);
#24224=ADVANCED_FACE('',(#2365),#1127,.T.);
#24225=ADVANCED_FACE('',(#2366),#1128,.T.);
#24226=ADVANCED_FACE('',(#2367),#1129,.T.);
#24227=ADVANCED_FACE('',(#2368),#1130,.T.);
#24228=ADVANCED_FACE('',(#2369),#1131,.T.);
#24229=ADVANCED_FACE('',(#2370),#1132,.T.);
#24230=ADVANCED_FACE('',(#2371),#1133,.T.);
#24231=ADVANCED_FACE('',(#2372),#1134,.T.);
#24232=ADVANCED_FACE('',(#2373),#1135,.T.);
#24233=ADVANCED_FACE('',(#2374),#1136,.T.);
#24234=ADVANCED_FACE('',(#2375),#1137,.T.);
#24235=ADVANCED_FACE('',(#2376),#1138,.T.);
#24236=ADVANCED_FACE('',(#2377),#1139,.T.);
#24237=ADVANCED_FACE('',(#2378),#1140,.T.);
#24238=ADVANCED_FACE('',(#2379),#1141,.T.);
#24239=ADVANCED_FACE('',(#2380),#1142,.T.);
#24240=ADVANCED_FACE('',(#2381),#1143,.T.);
#24241=ADVANCED_FACE('',(#2382),#1144,.T.);
#24242=ADVANCED_FACE('',(#2383),#1145,.T.);
#24243=ADVANCED_FACE('',(#2384),#1146,.T.);
#24244=ADVANCED_FACE('',(#2385),#1147,.T.);
#24245=ADVANCED_FACE('',(#2386),#1148,.T.);
#24246=ADVANCED_FACE('',(#2387),#1149,.T.);
#24247=ADVANCED_FACE('',(#2388),#1150,.T.);
#24248=ADVANCED_FACE('',(#2389),#1151,.T.);
#24249=ADVANCED_FACE('',(#2390),#1152,.T.);
#24250=ADVANCED_FACE('',(#2391),#1153,.T.);
#24251=ADVANCED_FACE('',(#2392),#1154,.T.);
#24252=ADVANCED_FACE('',(#2393),#1155,.T.);
#24253=ADVANCED_FACE('',(#2394),#1156,.T.);
#24254=ADVANCED_FACE('',(#2395),#514,.T.);
#24255=ADVANCED_FACE('',(#2396),#1157,.T.);
#24256=ADVANCED_FACE('',(#2397),#23589,.T.);
#24257=ADVANCED_FACE('',(#2398,#647),#515,.T.);
#24258=ADVANCED_FACE('',(#2399,#648),#1158,.T.);
#24259=ADVANCED_FACE('',(#2400),#516,.T.);
#24260=ADVANCED_FACE('',(#2401),#1159,.T.);
#24261=ADVANCED_FACE('',(#2402),#1160,.T.);
#24262=ADVANCED_FACE('',(#2403,#649),#1161,.F.);
#24263=ADVANCED_FACE('',(#2404),#1162,.T.);
#24264=ADVANCED_FACE('',(#2405),#1163,.T.);
#24265=ADVANCED_FACE('',(#2406),#1164,.T.);
#24266=ADVANCED_FACE('',(#2407),#1165,.T.);
#24267=ADVANCED_FACE('',(#2408),#1166,.T.);
#24268=ADVANCED_FACE('',(#2409),#1167,.T.);
#24269=ADVANCED_FACE('',(#2410),#1168,.T.);
#24270=ADVANCED_FACE('',(#2411),#1169,.T.);
#24271=ADVANCED_FACE('',(#2412),#1170,.T.);
#24272=ADVANCED_FACE('',(#2413),#1171,.T.);
#24273=ADVANCED_FACE('',(#2414),#1172,.T.);
#24274=ADVANCED_FACE('',(#2415),#1173,.T.);
#24275=ADVANCED_FACE('',(#2416),#1174,.T.);
#24276=ADVANCED_FACE('',(#2417),#1175,.T.);
#24277=ADVANCED_FACE('',(#2418),#1176,.T.);
#24278=ADVANCED_FACE('',(#2419),#1177,.T.);
#24279=ADVANCED_FACE('',(#2420),#1178,.T.);
#24280=ADVANCED_FACE('',(#2421),#1179,.T.);
#24281=ADVANCED_FACE('',(#2422),#1180,.T.);
#24282=ADVANCED_FACE('',(#2423),#1181,.T.);
#24283=ADVANCED_FACE('',(#2424),#1182,.T.);
#24284=ADVANCED_FACE('',(#2425),#1183,.T.);
#24285=ADVANCED_FACE('',(#2426),#1184,.T.);
#24286=ADVANCED_FACE('',(#2427),#1185,.T.);
#24287=ADVANCED_FACE('',(#2428),#1186,.T.);
#24288=ADVANCED_FACE('',(#2429),#1187,.T.);
#24289=ADVANCED_FACE('',(#2430),#1188,.T.);
#24290=ADVANCED_FACE('',(#2431),#1189,.T.);
#24291=ADVANCED_FACE('',(#2432),#1190,.T.);
#24292=ADVANCED_FACE('',(#2433),#1191,.T.);
#24293=ADVANCED_FACE('',(#2434),#1192,.T.);
#24294=ADVANCED_FACE('',(#2435),#1193,.T.);
#24295=ADVANCED_FACE('',(#2436),#1194,.T.);
#24296=ADVANCED_FACE('',(#2437),#1195,.T.);
#24297=ADVANCED_FACE('',(#2438),#1196,.T.);
#24298=ADVANCED_FACE('',(#2439),#1197,.T.);
#24299=ADVANCED_FACE('',(#2440),#1198,.T.);
#24300=ADVANCED_FACE('',(#2441),#1199,.T.);
#24301=ADVANCED_FACE('',(#2442),#1200,.T.);
#24302=ADVANCED_FACE('',(#2443),#1201,.T.);
#24303=ADVANCED_FACE('',(#2444),#1202,.T.);
#24304=ADVANCED_FACE('',(#2445),#1203,.T.);
#24305=ADVANCED_FACE('',(#2446),#1204,.T.);
#24306=ADVANCED_FACE('',(#2447),#1205,.T.);
#24307=ADVANCED_FACE('',(#2448),#1206,.T.);
#24308=ADVANCED_FACE('',(#2449),#1207,.T.);
#24309=ADVANCED_FACE('',(#2450),#1208,.T.);
#24310=ADVANCED_FACE('',(#2451),#1209,.T.);
#24311=ADVANCED_FACE('',(#2452),#1210,.T.);
#24312=ADVANCED_FACE('',(#2453),#1211,.T.);
#24313=ADVANCED_FACE('',(#2454),#1212,.T.);
#24314=ADVANCED_FACE('',(#2455),#1213,.T.);
#24315=ADVANCED_FACE('',(#2456),#1214,.T.);
#24316=ADVANCED_FACE('',(#2457),#1215,.T.);
#24317=ADVANCED_FACE('',(#2458),#1216,.T.);
#24318=ADVANCED_FACE('',(#2459),#1217,.T.);
#24319=ADVANCED_FACE('',(#2460),#1218,.T.);
#24320=ADVANCED_FACE('',(#2461),#1219,.T.);
#24321=ADVANCED_FACE('',(#2462),#1220,.T.);
#24322=ADVANCED_FACE('',(#2463),#1221,.T.);
#24323=ADVANCED_FACE('',(#2464),#1222,.T.);
#24324=ADVANCED_FACE('',(#2465),#1223,.T.);
#24325=ADVANCED_FACE('',(#2466),#1224,.T.);
#24326=ADVANCED_FACE('',(#2467),#1225,.T.);
#24327=ADVANCED_FACE('',(#2468),#1226,.T.);
#24328=ADVANCED_FACE('',(#2469),#1227,.T.);
#24329=ADVANCED_FACE('',(#2470),#1228,.T.);
#24330=ADVANCED_FACE('',(#2471),#1229,.T.);
#24331=ADVANCED_FACE('',(#2472),#1230,.T.);
#24332=ADVANCED_FACE('',(#2473),#1231,.T.);
#24333=ADVANCED_FACE('',(#2474),#1232,.T.);
#24334=ADVANCED_FACE('',(#2475),#1233,.T.);
#24335=ADVANCED_FACE('',(#2476,#650),#1234,.T.);
#24336=ADVANCED_FACE('',(#2477),#1235,.T.);
#24337=ADVANCED_FACE('',(#2478),#1236,.T.);
#24338=ADVANCED_FACE('',(#2479),#1237,.T.);
#24339=ADVANCED_FACE('',(#2480),#1238,.T.);
#24340=ADVANCED_FACE('',(#2481),#1239,.T.);
#24341=ADVANCED_FACE('',(#2482),#1240,.T.);
#24342=ADVANCED_FACE('',(#2483),#1241,.T.);
#24343=ADVANCED_FACE('',(#2484),#1242,.T.);
#24344=ADVANCED_FACE('',(#2485),#1243,.T.);
#24345=ADVANCED_FACE('',(#2486),#1244,.T.);
#24346=ADVANCED_FACE('',(#2487),#1245,.T.);
#24347=ADVANCED_FACE('',(#2488),#1246,.T.);
#24348=ADVANCED_FACE('',(#2489),#1247,.T.);
#24349=ADVANCED_FACE('',(#2490),#1248,.T.);
#24350=ADVANCED_FACE('',(#2491),#1249,.T.);
#24351=ADVANCED_FACE('',(#2492),#1250,.T.);
#24352=ADVANCED_FACE('',(#2493),#1251,.T.);
#24353=ADVANCED_FACE('',(#2494),#1252,.T.);
#24354=ADVANCED_FACE('',(#2495),#1253,.T.);
#24355=ADVANCED_FACE('',(#2496),#1254,.T.);
#24356=ADVANCED_FACE('',(#2497),#1255,.T.);
#24357=ADVANCED_FACE('',(#2498),#1256,.T.);
#24358=ADVANCED_FACE('',(#2499),#1257,.T.);
#24359=ADVANCED_FACE('',(#2500),#1258,.T.);
#24360=ADVANCED_FACE('',(#2501),#1259,.T.);
#24361=ADVANCED_FACE('',(#2502),#1260,.T.);
#24362=ADVANCED_FACE('',(#2503),#1261,.T.);
#24363=ADVANCED_FACE('',(#2504),#1262,.T.);
#24364=ADVANCED_FACE('',(#2505),#1263,.T.);
#24365=ADVANCED_FACE('',(#2506),#1264,.T.);
#24366=ADVANCED_FACE('',(#2507),#1265,.T.);
#24367=ADVANCED_FACE('',(#2508),#1266,.T.);
#24368=ADVANCED_FACE('',(#2509),#1267,.T.);
#24369=ADVANCED_FACE('',(#2510),#1268,.T.);
#24370=ADVANCED_FACE('',(#2511),#1269,.T.);
#24371=ADVANCED_FACE('',(#2512),#1270,.T.);
#24372=ADVANCED_FACE('',(#2513),#1271,.T.);
#24373=ADVANCED_FACE('',(#2514),#1272,.T.);
#24374=ADVANCED_FACE('',(#2515),#1273,.T.);
#24375=ADVANCED_FACE('',(#2516),#1274,.T.);
#24376=ADVANCED_FACE('',(#2517),#1275,.T.);
#24377=ADVANCED_FACE('',(#2518),#1276,.T.);
#24378=ADVANCED_FACE('',(#2519),#1277,.T.);
#24379=ADVANCED_FACE('',(#2520),#1278,.T.);
#24380=ADVANCED_FACE('',(#2521),#1279,.T.);
#24381=ADVANCED_FACE('',(#2522),#1280,.T.);
#24382=ADVANCED_FACE('',(#2523),#1281,.T.);
#24383=ADVANCED_FACE('',(#2524),#1282,.T.);
#24384=ADVANCED_FACE('',(#2525),#1283,.T.);
#24385=ADVANCED_FACE('',(#2526),#1284,.T.);
#24386=ADVANCED_FACE('',(#2527),#1285,.T.);
#24387=ADVANCED_FACE('',(#2528),#1286,.T.);
#24388=ADVANCED_FACE('',(#2529),#1287,.T.);
#24389=ADVANCED_FACE('',(#2530),#1288,.T.);
#24390=ADVANCED_FACE('',(#2531),#1289,.T.);
#24391=ADVANCED_FACE('',(#2532),#1290,.T.);
#24392=ADVANCED_FACE('',(#2533),#1291,.T.);
#24393=ADVANCED_FACE('',(#2534),#1292,.T.);
#24394=ADVANCED_FACE('',(#2535),#1293,.T.);
#24395=ADVANCED_FACE('',(#2536),#1294,.T.);
#24396=ADVANCED_FACE('',(#2537),#1295,.T.);
#24397=ADVANCED_FACE('',(#2538),#1296,.T.);
#24398=ADVANCED_FACE('',(#2539),#1297,.T.);
#24399=ADVANCED_FACE('',(#2540),#1298,.T.);
#24400=ADVANCED_FACE('',(#2541),#1299,.T.);
#24401=ADVANCED_FACE('',(#2542),#1300,.T.);
#24402=ADVANCED_FACE('',(#2543),#1301,.T.);
#24403=ADVANCED_FACE('',(#2544),#1302,.T.);
#24404=ADVANCED_FACE('',(#2545),#1303,.T.);
#24405=ADVANCED_FACE('',(#2546),#1304,.T.);
#24406=ADVANCED_FACE('',(#2547),#1305,.T.);
#24407=ADVANCED_FACE('',(#2548),#1306,.T.);
#24408=ADVANCED_FACE('',(#2549),#1307,.T.);
#24409=ADVANCED_FACE('',(#2550),#1308,.T.);
#24410=ADVANCED_FACE('',(#2551),#1309,.T.);
#24411=ADVANCED_FACE('',(#2552),#1310,.T.);
#24412=ADVANCED_FACE('',(#2553),#1311,.T.);
#24413=ADVANCED_FACE('',(#2554),#1312,.T.);
#24414=ADVANCED_FACE('',(#2555),#1313,.T.);
#24415=ADVANCED_FACE('',(#2556),#1314,.T.);
#24416=ADVANCED_FACE('',(#2557),#1315,.T.);
#24417=ADVANCED_FACE('',(#2558),#1316,.T.);
#24418=ADVANCED_FACE('',(#2559),#1317,.T.);
#24419=ADVANCED_FACE('',(#2560),#1318,.T.);
#24420=ADVANCED_FACE('',(#2561),#1319,.T.);
#24421=ADVANCED_FACE('',(#2562),#1320,.T.);
#24422=ADVANCED_FACE('',(#2563),#1321,.T.);
#24423=ADVANCED_FACE('',(#2564),#1322,.T.);
#24424=ADVANCED_FACE('',(#2565),#1323,.T.);
#24425=ADVANCED_FACE('',(#2566),#1324,.T.);
#24426=ADVANCED_FACE('',(#2567),#1325,.T.);
#24427=ADVANCED_FACE('',(#2568),#1326,.T.);
#24428=ADVANCED_FACE('',(#2569),#1327,.T.);
#24429=ADVANCED_FACE('',(#2570),#1328,.T.);
#24430=ADVANCED_FACE('',(#2571),#1329,.T.);
#24431=ADVANCED_FACE('',(#2572),#1330,.T.);
#24432=ADVANCED_FACE('',(#2573),#1331,.T.);
#24433=ADVANCED_FACE('',(#2574),#1332,.T.);
#24434=ADVANCED_FACE('',(#2575),#1333,.T.);
#24435=ADVANCED_FACE('',(#2576),#1334,.T.);
#24436=ADVANCED_FACE('',(#2577),#1335,.T.);
#24437=ADVANCED_FACE('',(#2578),#1336,.T.);
#24438=ADVANCED_FACE('',(#2579),#1337,.T.);
#24439=ADVANCED_FACE('',(#2580),#1338,.T.);
#24440=ADVANCED_FACE('',(#2581),#1339,.T.);
#24441=ADVANCED_FACE('',(#2582),#1340,.T.);
#24442=ADVANCED_FACE('',(#2583),#1341,.T.);
#24443=ADVANCED_FACE('',(#2584),#1342,.T.);
#24444=ADVANCED_FACE('',(#2585),#1343,.T.);
#24445=ADVANCED_FACE('',(#2586),#1344,.T.);
#24446=ADVANCED_FACE('',(#2587),#1345,.T.);
#24447=ADVANCED_FACE('',(#2588),#1346,.T.);
#24448=ADVANCED_FACE('',(#2589),#1347,.T.);
#24449=ADVANCED_FACE('',(#2590),#1348,.T.);
#24450=ADVANCED_FACE('',(#2591),#1349,.T.);
#24451=ADVANCED_FACE('',(#2592),#1350,.T.);
#24452=ADVANCED_FACE('',(#2593),#1351,.T.);
#24453=ADVANCED_FACE('',(#2594),#1352,.T.);
#24454=ADVANCED_FACE('',(#2595),#1353,.T.);
#24455=ADVANCED_FACE('',(#2596),#1354,.T.);
#24456=ADVANCED_FACE('',(#2597),#1355,.T.);
#24457=ADVANCED_FACE('',(#2598),#1356,.T.);
#24458=ADVANCED_FACE('',(#2599),#1357,.T.);
#24459=ADVANCED_FACE('',(#2600),#1358,.T.);
#24460=ADVANCED_FACE('',(#2601),#1359,.T.);
#24461=ADVANCED_FACE('',(#2602),#1360,.T.);
#24462=ADVANCED_FACE('',(#2603),#1361,.T.);
#24463=ADVANCED_FACE('',(#2604),#1362,.T.);
#24464=ADVANCED_FACE('',(#2605),#1363,.T.);
#24465=ADVANCED_FACE('',(#2606),#1364,.T.);
#24466=ADVANCED_FACE('',(#2607),#1365,.T.);
#24467=ADVANCED_FACE('',(#2608),#1366,.T.);
#24468=ADVANCED_FACE('',(#2609),#1367,.T.);
#24469=ADVANCED_FACE('',(#2610),#1368,.T.);
#24470=ADVANCED_FACE('',(#2611),#1369,.T.);
#24471=ADVANCED_FACE('',(#2612),#1370,.T.);
#24472=ADVANCED_FACE('',(#2613),#1371,.T.);
#24473=ADVANCED_FACE('',(#2614),#1372,.T.);
#24474=ADVANCED_FACE('',(#2615),#1373,.T.);
#24475=ADVANCED_FACE('',(#2616),#1374,.T.);
#24476=ADVANCED_FACE('',(#2617),#1375,.T.);
#24477=ADVANCED_FACE('',(#2618),#1376,.T.);
#24478=ADVANCED_FACE('',(#2619),#1377,.T.);
#24479=ADVANCED_FACE('',(#2620),#1378,.T.);
#24480=ADVANCED_FACE('',(#2621),#1379,.T.);
#24481=ADVANCED_FACE('',(#2622),#1380,.T.);
#24482=ADVANCED_FACE('',(#2623),#1381,.T.);
#24483=ADVANCED_FACE('',(#2624),#1382,.T.);
#24484=ADVANCED_FACE('',(#2625),#1383,.T.);
#24485=ADVANCED_FACE('',(#2626),#1384,.T.);
#24486=ADVANCED_FACE('',(#2627),#1385,.T.);
#24487=ADVANCED_FACE('',(#2628),#1386,.T.);
#24488=ADVANCED_FACE('',(#2629),#1387,.T.);
#24489=ADVANCED_FACE('',(#2630),#1388,.T.);
#24490=ADVANCED_FACE('',(#2631),#1389,.T.);
#24491=ADVANCED_FACE('',(#2632),#1390,.T.);
#24492=ADVANCED_FACE('',(#2633),#1391,.T.);
#24493=ADVANCED_FACE('',(#2634),#1392,.T.);
#24494=ADVANCED_FACE('',(#2635),#1393,.T.);
#24495=ADVANCED_FACE('',(#2636),#1394,.T.);
#24496=ADVANCED_FACE('',(#2637),#1395,.T.);
#24497=ADVANCED_FACE('',(#2638),#1396,.T.);
#24498=ADVANCED_FACE('',(#2639),#1397,.T.);
#24499=ADVANCED_FACE('',(#2640),#1398,.T.);
#24500=ADVANCED_FACE('',(#2641),#1399,.T.);
#24501=ADVANCED_FACE('',(#2642),#1400,.T.);
#24502=ADVANCED_FACE('',(#2643),#1401,.T.);
#24503=ADVANCED_FACE('',(#2644),#1402,.T.);
#24504=ADVANCED_FACE('',(#2645),#1403,.T.);
#24505=ADVANCED_FACE('',(#2646),#1404,.T.);
#24506=ADVANCED_FACE('',(#2647),#1405,.T.);
#24507=ADVANCED_FACE('',(#2648),#1406,.T.);
#24508=ADVANCED_FACE('',(#2649),#1407,.T.);
#24509=ADVANCED_FACE('',(#2650),#1408,.T.);
#24510=ADVANCED_FACE('',(#2651),#1409,.T.);
#24511=ADVANCED_FACE('',(#2652),#1410,.T.);
#24512=ADVANCED_FACE('',(#2653),#1411,.T.);
#24513=ADVANCED_FACE('',(#2654),#1412,.T.);
#24514=ADVANCED_FACE('',(#2655),#1413,.T.);
#24515=ADVANCED_FACE('',(#2656),#1414,.T.);
#24516=ADVANCED_FACE('',(#2657),#1415,.T.);
#24517=ADVANCED_FACE('',(#2658),#1416,.T.);
#24518=ADVANCED_FACE('',(#2659),#1417,.T.);
#24519=ADVANCED_FACE('',(#2660),#1418,.T.);
#24520=ADVANCED_FACE('',(#2661),#1419,.T.);
#24521=ADVANCED_FACE('',(#2662),#1420,.T.);
#24522=ADVANCED_FACE('',(#2663),#1421,.T.);
#24523=ADVANCED_FACE('',(#2664),#1422,.T.);
#24524=ADVANCED_FACE('',(#2665),#1423,.T.);
#24525=ADVANCED_FACE('',(#2666),#1424,.T.);
#24526=ADVANCED_FACE('',(#2667),#1425,.T.);
#24527=ADVANCED_FACE('',(#2668),#1426,.T.);
#24528=ADVANCED_FACE('',(#2669),#1427,.T.);
#24529=ADVANCED_FACE('',(#2670),#1428,.T.);
#24530=ADVANCED_FACE('',(#2671),#1429,.T.);
#24531=ADVANCED_FACE('',(#2672),#1430,.T.);
#24532=ADVANCED_FACE('',(#2673),#1431,.T.);
#24533=ADVANCED_FACE('',(#2674),#1432,.T.);
#24534=ADVANCED_FACE('',(#2675),#1433,.T.);
#24535=ADVANCED_FACE('',(#2676),#1434,.T.);
#24536=ADVANCED_FACE('',(#2677),#1435,.T.);
#24537=ADVANCED_FACE('',(#2678),#1436,.T.);
#24538=ADVANCED_FACE('',(#2679),#1437,.T.);
#24539=ADVANCED_FACE('',(#2680),#1438,.T.);
#24540=ADVANCED_FACE('',(#2681),#1439,.T.);
#24541=ADVANCED_FACE('',(#2682),#1440,.T.);
#24542=ADVANCED_FACE('',(#2683),#1441,.T.);
#24543=ADVANCED_FACE('',(#2684),#1442,.T.);
#24544=ADVANCED_FACE('',(#2685),#1443,.T.);
#24545=ADVANCED_FACE('',(#2686),#1444,.T.);
#24546=ADVANCED_FACE('',(#2687),#1445,.T.);
#24547=ADVANCED_FACE('',(#2688),#1446,.T.);
#24548=ADVANCED_FACE('',(#2689),#1447,.T.);
#24549=ADVANCED_FACE('',(#2690),#1448,.T.);
#24550=ADVANCED_FACE('',(#2691),#1449,.T.);
#24551=ADVANCED_FACE('',(#2692),#1450,.T.);
#24552=ADVANCED_FACE('',(#2693),#1451,.T.);
#24553=ADVANCED_FACE('',(#2694),#1452,.T.);
#24554=ADVANCED_FACE('',(#2695),#1453,.T.);
#24555=ADVANCED_FACE('',(#2696),#1454,.T.);
#24556=ADVANCED_FACE('',(#2697),#1455,.T.);
#24557=ADVANCED_FACE('',(#2698),#1456,.T.);
#24558=ADVANCED_FACE('',(#2699),#1457,.T.);
#24559=ADVANCED_FACE('',(#2700),#1458,.T.);
#24560=ADVANCED_FACE('',(#2701),#1459,.T.);
#24561=ADVANCED_FACE('',(#2702),#1460,.T.);
#24562=ADVANCED_FACE('',(#2703),#1461,.T.);
#24563=ADVANCED_FACE('',(#2704),#1462,.T.);
#24564=ADVANCED_FACE('',(#2705),#1463,.T.);
#24565=ADVANCED_FACE('',(#2706),#1464,.T.);
#24566=ADVANCED_FACE('',(#2707),#1465,.T.);
#24567=ADVANCED_FACE('',(#2708),#1466,.T.);
#24568=ADVANCED_FACE('',(#2709),#1467,.T.);
#24569=ADVANCED_FACE('',(#2710),#1468,.T.);
#24570=ADVANCED_FACE('',(#2711),#1469,.T.);
#24571=ADVANCED_FACE('',(#2712),#1470,.T.);
#24572=ADVANCED_FACE('',(#2713),#1471,.T.);
#24573=ADVANCED_FACE('',(#2714),#1472,.T.);
#24574=ADVANCED_FACE('',(#2715),#1473,.T.);
#24575=ADVANCED_FACE('',(#2716),#1474,.T.);
#24576=ADVANCED_FACE('',(#2717),#1475,.T.);
#24577=ADVANCED_FACE('',(#2718),#1476,.T.);
#24578=ADVANCED_FACE('',(#2719),#1477,.T.);
#24579=ADVANCED_FACE('',(#2720),#1478,.T.);
#24580=ADVANCED_FACE('',(#2721),#1479,.T.);
#24581=ADVANCED_FACE('',(#2722),#1480,.T.);
#24582=ADVANCED_FACE('',(#2723),#1481,.T.);
#24583=ADVANCED_FACE('',(#2724),#1482,.T.);
#24584=ADVANCED_FACE('',(#2725),#1483,.T.);
#24585=ADVANCED_FACE('',(#2726),#1484,.T.);
#24586=ADVANCED_FACE('',(#2727),#1485,.T.);
#24587=ADVANCED_FACE('',(#2728),#1486,.T.);
#24588=ADVANCED_FACE('',(#2729),#1487,.T.);
#24589=ADVANCED_FACE('',(#2730),#1488,.T.);
#24590=ADVANCED_FACE('',(#2731),#1489,.T.);
#24591=ADVANCED_FACE('',(#2732),#1490,.T.);
#24592=ADVANCED_FACE('',(#2733),#1491,.T.);
#24593=ADVANCED_FACE('',(#2734),#1492,.T.);
#24594=ADVANCED_FACE('',(#2735),#1493,.T.);
#24595=ADVANCED_FACE('',(#2736),#1494,.T.);
#24596=ADVANCED_FACE('',(#2737),#1495,.T.);
#24597=ADVANCED_FACE('',(#2738),#1496,.T.);
#24598=ADVANCED_FACE('',(#2739),#1497,.T.);
#24599=ADVANCED_FACE('',(#2740),#517,.T.);
#24600=ADVANCED_FACE('',(#2741),#1498,.T.);
#24601=ADVANCED_FACE('',(#2742),#518,.T.);
#24602=ADVANCED_FACE('',(#2743),#1499,.T.);
#24603=ADVANCED_FACE('',(#2744),#1500,.F.);
#24604=ADVANCED_FACE('',(#2745),#1501,.F.);
#24605=ADVANCED_FACE('',(#2746),#1502,.F.);
#24606=ADVANCED_FACE('',(#2747),#1503,.F.);
#24607=ADVANCED_FACE('',(#2748),#1504,.F.);
#24608=ADVANCED_FACE('',(#2749),#1505,.F.);
#24609=ADVANCED_FACE('',(#2750),#1506,.F.);
#24610=ADVANCED_FACE('',(#2751),#1507,.F.);
#24611=ADVANCED_FACE('',(#2752),#1508,.F.);
#24612=ADVANCED_FACE('',(#2753),#1509,.F.);
#24613=ADVANCED_FACE('',(#2754),#519,.F.);
#24614=ADVANCED_FACE('',(#2755),#520,.F.);
#24615=ADVANCED_FACE('',(#2756),#521,.T.);
#24616=ADVANCED_FACE('',(#2757),#522,.T.);
#24617=ADVANCED_FACE('',(#2758,#651,#652,#653,#654),#1510,.T.);
#24618=ADVANCED_FACE('',(#2759,#655,#656),#1511,.F.);
#24619=ADVANCED_FACE('',(#2760),#23590,.T.);
#24620=ADVANCED_FACE('',(#2761,#657),#1512,.T.);
#24621=ADVANCED_FACE('',(#2762),#23591,.T.);
#24622=ADVANCED_FACE('',(#2763),#523,.F.);
#24623=ADVANCED_FACE('',(#2764,#658),#1513,.T.);
#24624=ADVANCED_FACE('',(#2765),#524,.T.);
#24625=ADVANCED_FACE('',(#2766,#659),#1514,.T.);
#24626=ADVANCED_FACE('',(#2767),#525,.F.);
#24627=ADVANCED_FACE('',(#2768,#660),#1515,.T.);
#24628=ADVANCED_FACE('',(#2769),#23592,.F.);
#24629=ADVANCED_FACE('',(#2770),#1516,.T.);
#24630=ADVANCED_FACE('',(#2771),#23593,.F.);
#24631=ADVANCED_FACE('',(#2772),#1517,.T.);
#24632=ADVANCED_FACE('',(#2773),#1518,.T.);
#24633=ADVANCED_FACE('',(#2774),#526,.F.);
#24634=ADVANCED_FACE('',(#2775),#1519,.T.);
#24635=ADVANCED_FACE('',(#2776),#1520,.T.);
#24636=ADVANCED_FACE('',(#2777),#23594,.F.);
#24637=ADVANCED_FACE('',(#2778),#1521,.T.);
#24638=ADVANCED_FACE('',(#2779,#661,#662),#1522,.F.);
#24639=ADVANCED_FACE('',(#2780),#527,.T.);
#24640=ADVANCED_FACE('',(#2781),#23595,.F.);
#24641=ADVANCED_FACE('',(#2782),#528,.F.);
#24642=ADVANCED_FACE('',(#2783),#23596,.F.);
#24643=ADVANCED_FACE('',(#2784,#663,#664),#1523,.T.);
#24644=ADVANCED_FACE('',(#2785),#23597,.F.);
#24645=ADVANCED_FACE('',(#2786),#529,.F.);
#24646=ADVANCED_FACE('',(#2787),#23598,.F.);
#24647=ADVANCED_FACE('',(#2788),#1524,.T.);
#24648=ADVANCED_FACE('',(#2789),#1525,.T.);
#24649=ADVANCED_FACE('',(#2790),#1526,.T.);
#24650=ADVANCED_FACE('',(#2791),#1527,.T.);
#24651=ADVANCED_FACE('',(#2792),#1528,.T.);
#24652=ADVANCED_FACE('',(#2793),#1529,.T.);
#24653=ADVANCED_FACE('',(#2794),#1530,.T.);
#24654=ADVANCED_FACE('',(#2795),#1531,.T.);
#24655=ADVANCED_FACE('',(#2796),#1532,.T.);
#24656=ADVANCED_FACE('',(#2797),#1533,.T.);
#24657=ADVANCED_FACE('',(#2798),#1534,.T.);
#24658=ADVANCED_FACE('',(#2799),#1535,.T.);
#24659=ADVANCED_FACE('',(#2800),#1536,.T.);
#24660=ADVANCED_FACE('',(#2801),#1537,.T.);
#24661=ADVANCED_FACE('',(#2802),#1538,.T.);
#24662=ADVANCED_FACE('',(#2803),#1539,.T.);
#24663=ADVANCED_FACE('',(#2804),#1540,.T.);
#24664=ADVANCED_FACE('',(#2805),#1541,.F.);
#24665=ADVANCED_FACE('',(#2806),#233,.T.);
#24666=ADVANCED_FACE('',(#2807),#530,.T.);
#24667=ADVANCED_FACE('',(#2808),#234,.T.);
#24668=ADVANCED_FACE('',(#2809),#531,.T.);
#24669=ADVANCED_FACE('',(#2810),#1542,.T.);
#24670=ADVANCED_FACE('',(#2811),#1543,.T.);
#24671=ADVANCED_FACE('',(#2812),#1544,.T.);
#24672=ADVANCED_FACE('',(#2813),#1545,.T.);
#24673=ADVANCED_FACE('',(#2814),#1546,.T.);
#24674=ADVANCED_FACE('',(#2815),#1547,.T.);
#24675=ADVANCED_FACE('',(#2816),#1548,.T.);
#24676=ADVANCED_FACE('',(#2817),#1549,.T.);
#24677=ADVANCED_FACE('',(#2818),#1550,.T.);
#24678=ADVANCED_FACE('',(#2819),#1551,.T.);
#24679=ADVANCED_FACE('',(#2820),#1552,.T.);
#24680=ADVANCED_FACE('',(#2821),#1553,.T.);
#24681=ADVANCED_FACE('',(#2822),#1554,.T.);
#24682=ADVANCED_FACE('',(#2823),#1555,.T.);
#24683=ADVANCED_FACE('',(#2824),#1556,.T.);
#24684=ADVANCED_FACE('',(#2825),#1557,.T.);
#24685=ADVANCED_FACE('',(#2826),#1558,.T.);
#24686=ADVANCED_FACE('',(#2827),#1559,.T.);
#24687=ADVANCED_FACE('',(#2828),#1560,.T.);
#24688=ADVANCED_FACE('',(#2829),#1561,.T.);
#24689=ADVANCED_FACE('',(#2830),#1562,.T.);
#24690=ADVANCED_FACE('',(#2831,#665),#1563,.F.);
#24691=ADVANCED_FACE('',(#2832),#1564,.T.);
#24692=ADVANCED_FACE('',(#2833),#1565,.T.);
#24693=ADVANCED_FACE('',(#2834),#1566,.T.);
#24694=ADVANCED_FACE('',(#2835),#1567,.T.);
#24695=ADVANCED_FACE('',(#2836),#1568,.T.);
#24696=ADVANCED_FACE('',(#2837),#1569,.T.);
#24697=ADVANCED_FACE('',(#2838),#1570,.F.);
#24698=ADVANCED_FACE('',(#2839),#1571,.F.);
#24699=ADVANCED_FACE('',(#2840),#1572,.F.);
#24700=ADVANCED_FACE('',(#2841,#666),#1573,.T.);
#24701=ADVANCED_FACE('',(#2842),#1574,.F.);
#24702=ADVANCED_FACE('',(#2843),#1575,.F.);
#24703=ADVANCED_FACE('',(#2844),#1576,.F.);
#24704=ADVANCED_FACE('',(#2845),#1577,.F.);
#24705=ADVANCED_FACE('',(#2846),#23599,.T.);
#24706=ADVANCED_FACE('',(#2847),#1578,.T.);
#24707=ADVANCED_FACE('',(#2848),#1579,.T.);
#24708=ADVANCED_FACE('',(#2849),#1580,.T.);
#24709=ADVANCED_FACE('',(#2850),#1581,.T.);
#24710=ADVANCED_FACE('',(#2851),#23600,.T.);
#24711=ADVANCED_FACE('',(#2852),#532,.T.);
#24712=ADVANCED_FACE('',(#2853,#667),#1582,.T.);
#24713=ADVANCED_FACE('',(#2854),#533,.T.);
#24714=ADVANCED_FACE('',(#2855),#534,.F.);
#24715=ADVANCED_FACE('',(#2856,#668),#1583,.T.);
#24716=ADVANCED_FACE('',(#2857,#669),#1584,.T.);
#24717=ADVANCED_FACE('',(#2858),#535,.F.);
#24718=ADVANCED_FACE('',(#2859),#536,.F.);
#24719=ADVANCED_FACE('',(#2860,#670),#1585,.T.);
#24720=ADVANCED_FACE('',(#2861),#537,.T.);
#24721=ADVANCED_FACE('',(#2862,#671),#1586,.T.);
#24722=ADVANCED_FACE('',(#2863),#538,.F.);
#24723=ADVANCED_FACE('',(#2864,#672),#1587,.T.);
#24724=ADVANCED_FACE('',(#2865),#539,.F.);
#24725=ADVANCED_FACE('',(#2866,#673),#1588,.T.);
#24726=ADVANCED_FACE('',(#2867),#540,.T.);
#24727=ADVANCED_FACE('',(#2868),#541,.T.);
#24728=ADVANCED_FACE('',(#2869),#542,.T.);
#24729=ADVANCED_FACE('',(#2870),#543,.T.);
#24730=ADVANCED_FACE('',(#2871),#544,.T.);
#24731=ADVANCED_FACE('',(#2872),#545,.T.);
#24732=ADVANCED_FACE('',(#2873),#546,.T.);
#24733=ADVANCED_FACE('',(#2874),#547,.T.);
#24734=ADVANCED_FACE('',(#2875),#548,.T.);
#24735=ADVANCED_FACE('',(#2876),#549,.T.);
#24736=ADVANCED_FACE('',(#2877),#550,.T.);
#24737=ADVANCED_FACE('',(#2878),#551,.T.);
#24738=ADVANCED_FACE('',(#2879),#552,.T.);
#24739=ADVANCED_FACE('',(#2880),#553,.T.);
#24740=ADVANCED_FACE('',(#2881),#554,.T.);
#24741=ADVANCED_FACE('',(#2882),#555,.T.);
#24742=ADVANCED_FACE('',(#2883),#556,.T.);
#24743=ADVANCED_FACE('',(#2884),#557,.T.);
#24744=ADVANCED_FACE('',(#2885),#558,.T.);
#24745=ADVANCED_FACE('',(#2886),#559,.T.);
#24746=ADVANCED_FACE('',(#2887),#560,.T.);
#24747=ADVANCED_FACE('',(#2888),#561,.T.);
#24748=ADVANCED_FACE('',(#2889),#562,.T.);
#24749=ADVANCED_FACE('',(#2890),#563,.T.);
#24750=ADVANCED_FACE('',(#2891),#564,.T.);
#24751=ADVANCED_FACE('',(#2892),#565,.T.);
#24752=ADVANCED_FACE('',(#2893),#566,.T.);
#24753=ADVANCED_FACE('',(#2894),#567,.T.);
#24754=ADVANCED_FACE('',(#2895),#568,.T.);
#24755=ADVANCED_FACE('',(#2896),#569,.T.);
#24756=ADVANCED_FACE('',(#2897),#570,.T.);
#24757=ADVANCED_FACE('',(#2898),#571,.T.);
#24758=ADVANCED_FACE('',(#2899),#572,.T.);
#24759=ADVANCED_FACE('',(#2900),#573,.T.);
#24760=ADVANCED_FACE('',(#2901),#574,.T.);
#24761=ADVANCED_FACE('',(#2902),#575,.T.);
#24762=ADVANCED_FACE('',(#2903),#576,.T.);
#24763=ADVANCED_FACE('',(#2904),#577,.T.);
#24764=ADVANCED_FACE('',(#2905),#578,.T.);
#24765=ADVANCED_FACE('',(#2906),#579,.T.);
#24766=ADVANCED_FACE('',(#2907),#580,.T.);
#24767=ADVANCED_FACE('',(#2908),#1589,.F.);
#24768=ADVANCED_FACE('',(#2909),#398,.F.);
#24769=ADVANCED_FACE('',(#2910),#1590,.T.);
#24770=ADVANCED_FACE('',(#2911),#581,.T.);
#24771=ADVANCED_FACE('',(#2912),#399,.F.);
#24772=ADVANCED_FACE('',(#2913),#1591,.F.);
#24773=ADVANCED_FACE('',(#2914),#1592,.T.);
#24774=ADVANCED_FACE('',(#2915),#1593,.F.);
#24775=ADVANCED_FACE('',(#2916),#1594,.F.);
#24776=ADVANCED_FACE('',(#2917),#1595,.F.);
#24777=ADVANCED_FACE('',(#2918),#1596,.T.);
#24778=ADVANCED_FACE('',(#2919),#1597,.F.);
#24779=ADVANCED_FACE('',(#2920),#1598,.F.);
#24780=ADVANCED_FACE('',(#2921),#1599,.F.);
#24781=ADVANCED_FACE('',(#2922),#1600,.T.);
#24782=ADVANCED_FACE('',(#2923),#1601,.F.);
#24783=ADVANCED_FACE('',(#2924),#1602,.F.);
#24784=ADVANCED_FACE('',(#2925),#1603,.F.);
#24785=ADVANCED_FACE('',(#2926),#1604,.T.);
#24786=ADVANCED_FACE('',(#2927),#1605,.F.);
#24787=ADVANCED_FACE('',(#2928),#1606,.F.);
#24788=ADVANCED_FACE('',(#2929),#1607,.F.);
#24789=ADVANCED_FACE('',(#2930),#1608,.T.);
#24790=ADVANCED_FACE('',(#2931),#1609,.F.);
#24791=ADVANCED_FACE('',(#2932),#1610,.F.);
#24792=ADVANCED_FACE('',(#2933),#1611,.F.);
#24793=ADVANCED_FACE('',(#2934),#1612,.T.);
#24794=ADVANCED_FACE('',(#2935),#1613,.F.);
#24795=ADVANCED_FACE('',(#2936),#1614,.F.);
#24796=ADVANCED_FACE('',(#2937),#1615,.F.);
#24797=ADVANCED_FACE('',(#2938),#1616,.T.);
#24798=ADVANCED_FACE('',(#2939),#1617,.F.);
#24799=ADVANCED_FACE('',(#2940),#1618,.F.);
#24800=ADVANCED_FACE('',(#2941),#1619,.F.);
#24801=ADVANCED_FACE('',(#2942),#1620,.T.);
#24802=ADVANCED_FACE('',(#2943),#1621,.F.);
#24803=ADVANCED_FACE('',(#2944),#1622,.F.);
#24804=ADVANCED_FACE('',(#2945),#1623,.F.);
#24805=ADVANCED_FACE('',(#2946),#1624,.T.);
#24806=ADVANCED_FACE('',(#2947),#1625,.F.);
#24807=ADVANCED_FACE('',(#2948),#1626,.F.);
#24808=ADVANCED_FACE('',(#2949),#1627,.F.);
#24809=ADVANCED_FACE('',(#2950),#1628,.T.);
#24810=ADVANCED_FACE('',(#2951),#1629,.F.);
#24811=ADVANCED_FACE('',(#2952),#1630,.F.);
#24812=ADVANCED_FACE('',(#2953),#1631,.F.);
#24813=ADVANCED_FACE('',(#2954),#1632,.T.);
#24814=ADVANCED_FACE('',(#2955),#1633,.F.);
#24815=ADVANCED_FACE('',(#2956),#1634,.F.);
#24816=ADVANCED_FACE('',(#2957),#1635,.F.);
#24817=ADVANCED_FACE('',(#2958),#1636,.T.);
#24818=ADVANCED_FACE('',(#2959),#1637,.F.);
#24819=ADVANCED_FACE('',(#2960),#1638,.F.);
#24820=ADVANCED_FACE('',(#2961),#1639,.F.);
#24821=ADVANCED_FACE('',(#2962),#1640,.T.);
#24822=ADVANCED_FACE('',(#2963),#1641,.F.);
#24823=ADVANCED_FACE('',(#2964),#1642,.F.);
#24824=ADVANCED_FACE('',(#2965),#1643,.F.);
#24825=ADVANCED_FACE('',(#2966),#1644,.T.);
#24826=ADVANCED_FACE('',(#2967),#1645,.F.);
#24827=ADVANCED_FACE('',(#2968),#1646,.F.);
#24828=ADVANCED_FACE('',(#2969),#1647,.F.);
#24829=ADVANCED_FACE('',(#2970),#1648,.T.);
#24830=ADVANCED_FACE('',(#2971),#1649,.F.);
#24831=ADVANCED_FACE('',(#2972),#1650,.F.);
#24832=ADVANCED_FACE('',(#2973),#1651,.F.);
#24833=ADVANCED_FACE('',(#2974),#1652,.T.);
#24834=ADVANCED_FACE('',(#2975),#1653,.F.);
#24835=ADVANCED_FACE('',(#2976),#1654,.F.);
#24836=ADVANCED_FACE('',(#2977),#1655,.F.);
#24837=ADVANCED_FACE('',(#2978),#1656,.T.);
#24838=ADVANCED_FACE('',(#2979),#1657,.F.);
#24839=ADVANCED_FACE('',(#2980),#1658,.F.);
#24840=ADVANCED_FACE('',(#2981),#1659,.F.);
#24841=ADVANCED_FACE('',(#2982),#1660,.T.);
#24842=ADVANCED_FACE('',(#2983),#1661,.F.);
#24843=ADVANCED_FACE('',(#2984),#1662,.F.);
#24844=ADVANCED_FACE('',(#2985),#1663,.F.);
#24845=ADVANCED_FACE('',(#2986),#1664,.T.);
#24846=ADVANCED_FACE('',(#2987),#1665,.F.);
#24847=ADVANCED_FACE('',(#2988),#1666,.F.);
#24848=ADVANCED_FACE('',(#2989),#1667,.F.);
#24849=ADVANCED_FACE('',(#2990),#1668,.T.);
#24850=ADVANCED_FACE('',(#2991),#1669,.F.);
#24851=ADVANCED_FACE('',(#2992),#1670,.F.);
#24852=ADVANCED_FACE('',(#2993),#1671,.F.);
#24853=ADVANCED_FACE('',(#2994),#1672,.T.);
#24854=ADVANCED_FACE('',(#2995),#1673,.F.);
#24855=ADVANCED_FACE('',(#2996),#1674,.F.);
#24856=ADVANCED_FACE('',(#2997),#1675,.F.);
#24857=ADVANCED_FACE('',(#2998),#1676,.T.);
#24858=ADVANCED_FACE('',(#2999),#1677,.F.);
#24859=ADVANCED_FACE('',(#3000),#1678,.F.);
#24860=ADVANCED_FACE('',(#3001),#1679,.F.);
#24861=ADVANCED_FACE('',(#3002),#1680,.T.);
#24862=ADVANCED_FACE('',(#3003),#1681,.F.);
#24863=ADVANCED_FACE('',(#3004),#1682,.F.);
#24864=ADVANCED_FACE('',(#3005),#1683,.F.);
#24865=ADVANCED_FACE('',(#3006),#1684,.T.);
#24866=ADVANCED_FACE('',(#3007),#1685,.F.);
#24867=ADVANCED_FACE('',(#3008),#1686,.F.);
#24868=ADVANCED_FACE('',(#3009),#1687,.F.);
#24869=ADVANCED_FACE('',(#3010),#1688,.T.);
#24870=ADVANCED_FACE('',(#3011),#1689,.F.);
#24871=ADVANCED_FACE('',(#3012),#1690,.F.);
#24872=ADVANCED_FACE('',(#3013),#1691,.F.);
#24873=ADVANCED_FACE('',(#3014),#1692,.T.);
#24874=ADVANCED_FACE('',(#3015),#1693,.F.);
#24875=ADVANCED_FACE('',(#3016),#1694,.F.);
#24876=ADVANCED_FACE('',(#3017),#1695,.F.);
#24877=ADVANCED_FACE('',(#3018),#1696,.T.);
#24878=ADVANCED_FACE('',(#3019),#1697,.F.);
#24879=ADVANCED_FACE('',(#3020),#1698,.F.);
#24880=ADVANCED_FACE('',(#3021),#1699,.F.);
#24881=ADVANCED_FACE('',(#3022),#1700,.T.);
#24882=ADVANCED_FACE('',(#3023),#1701,.F.);
#24883=ADVANCED_FACE('',(#3024),#1702,.F.);
#24884=ADVANCED_FACE('',(#3025),#1703,.F.);
#24885=ADVANCED_FACE('',(#3026),#1704,.T.);
#24886=ADVANCED_FACE('',(#3027),#1705,.F.);
#24887=ADVANCED_FACE('',(#3028),#1706,.F.);
#24888=ADVANCED_FACE('',(#3029),#1707,.F.);
#24889=ADVANCED_FACE('',(#3030),#1708,.T.);
#24890=ADVANCED_FACE('',(#3031),#1709,.F.);
#24891=ADVANCED_FACE('',(#3032),#1710,.F.);
#24892=ADVANCED_FACE('',(#3033),#1711,.F.);
#24893=ADVANCED_FACE('',(#3034),#1712,.T.);
#24894=ADVANCED_FACE('',(#3035),#1713,.F.);
#24895=ADVANCED_FACE('',(#3036),#1714,.F.);
#24896=ADVANCED_FACE('',(#3037),#1715,.F.);
#24897=ADVANCED_FACE('',(#3038),#1716,.T.);
#24898=ADVANCED_FACE('',(#3039),#1717,.F.);
#24899=ADVANCED_FACE('',(#3040),#1718,.F.);
#24900=ADVANCED_FACE('',(#3041),#1719,.F.);
#24901=ADVANCED_FACE('',(#3042),#1720,.T.);
#24902=ADVANCED_FACE('',(#3043),#1721,.F.);
#24903=ADVANCED_FACE('',(#3044),#1722,.F.);
#24904=ADVANCED_FACE('',(#3045),#1723,.F.);
#24905=ADVANCED_FACE('',(#3046),#1724,.T.);
#24906=ADVANCED_FACE('',(#3047),#1725,.F.);
#24907=ADVANCED_FACE('',(#3048),#1726,.F.);
#24908=ADVANCED_FACE('',(#3049),#1727,.F.);
#24909=ADVANCED_FACE('',(#3050),#1728,.T.);
#24910=ADVANCED_FACE('',(#3051),#1729,.F.);
#24911=ADVANCED_FACE('',(#3052),#1730,.F.);
#24912=ADVANCED_FACE('',(#3053),#1731,.F.);
#24913=ADVANCED_FACE('',(#3054),#1732,.T.);
#24914=ADVANCED_FACE('',(#3055),#1733,.F.);
#24915=ADVANCED_FACE('',(#3056),#1734,.F.);
#24916=ADVANCED_FACE('',(#3057),#1735,.F.);
#24917=ADVANCED_FACE('',(#3058),#1736,.F.);
#24918=ADVANCED_FACE('',(#3059),#1737,.F.);
#24919=ADVANCED_FACE('',(#3060),#1738,.F.);
#24920=ADVANCED_FACE('',(#3061),#1739,.F.);
#24921=ADVANCED_FACE('',(#3062),#1740,.F.);
#24922=ADVANCED_FACE('',(#3063),#1741,.F.);
#24923=ADVANCED_FACE('',(#3064),#1742,.T.);
#24924=ADVANCED_FACE('',(#3065),#23601,.T.);
#24925=ADVANCED_FACE('',(#3066),#582,.T.);
#24926=ADVANCED_FACE('',(#3067),#23602,.F.);
#24927=ADVANCED_FACE('',(#3068),#583,.T.);
#24928=ADVANCED_FACE('',(#3069,#674),#1743,.T.);
#24929=ADVANCED_FACE('',(#3070,#675,#676,#677,#678,#679,#680,#681,#682,
#683,#684,#685,#686,#687,#688,#689,#690,#691,#692,#693,#694,#695,#696,#697,
#698,#699,#700,#701,#702,#703,#704,#705,#706,#707,#708,#709),#584,.T.);
#24930=ADVANCED_FACE('',(#3071),#23603,.T.);
#24931=ADVANCED_FACE('',(#3072,#710),#1744,.T.);
#24932=ADVANCED_FACE('',(#3073),#1745,.T.);
#24933=ADVANCED_FACE('',(#3074),#23604,.T.);
#24934=ADVANCED_FACE('',(#3075),#585,.T.);
#24935=ADVANCED_FACE('',(#3076),#23605,.T.);
#24936=ADVANCED_FACE('',(#3077),#1746,.T.);
#24937=CLOSED_SHELL('',(#23606,#23607,#23608,#23609,#23610,#23611,#23612,
#23613,#23614,#23615,#23616,#23617,#23618,#23619,#23620,#23621,#23622,#23623,
#23624,#23625,#23626,#23627,#23628,#23629,#23630,#23631,#23632,#23633,#23634,
#23635,#23636,#23637,#23638,#23639,#23640,#23641,#23642,#23643,#23644,#23645,
#23646,#23647,#23648,#23649,#23650,#23651,#23652,#23653,#23654,#23655,#23656,
#23657,#23658,#23659,#23660,#23661,#23662,#23663,#23664,#23665,#23666,#23667,
#23668,#23669,#23670,#23671,#23672,#23673,#23674,#23675,#23676,#23677,#23678,
#23679,#23680,#23681,#23682,#23683,#23684,#23685,#23686,#23687,#23688,#23689,
#23690,#23691,#23692,#23693,#23694,#23695,#23696,#23697,#23698,#23699,#23700,
#23701,#23702,#23703,#23704,#23705,#23706,#23707,#23708,#23709,#23710,#23711,
#23712,#23713,#23714,#23715,#23716,#23717,#23718,#23719,#23720,#23721,#23722,
#23723,#23724,#23725,#23726,#23727,#23728,#23729,#23730,#23731,#23732,#23733,
#23734,#23735,#23736,#23737,#23738,#23739,#23740,#23741,#23742,#23743,#23744,
#23745,#23746,#23747,#23748,#23749,#23750,#23751,#23752,#23753,#23754,#23755,
#23756,#23757,#23758,#23759,#23760,#23761,#23762,#23763,#23764,#23765,#23766,
#23767,#23768,#23769,#23770,#23771,#23772,#23773,#23774,#23775,#23776,#23777,
#23778,#23779,#23780,#23781));
#24938=CLOSED_SHELL('',(#23782,#23783,#23784,#23785,#23786,#23787,#23788,
#23789,#23790,#23791,#23792,#23793,#23794,#23795,#23796,#23797,#23798,#23799,
#23800,#23801,#23802,#23803,#23804,#23805,#23806,#23807,#23808,#23809,#23810,
#23811,#23812,#23813,#23814,#23815,#23816,#23817,#23818,#23819,#23820,#23821,
#23822,#23823,#23824,#23825,#23826,#23827,#23828,#23829,#23830,#23831,#23832,
#23833));
#24939=CLOSED_SHELL('',(#23834,#23835,#23836,#23837,#23838,#23839,#23840,
#23841,#23842,#23843,#23844,#23845,#23846,#23847,#23848,#23849,#23850,#23851,
#23852,#23853,#23854,#23855,#23856,#23857,#23858,#23859,#23860,#23861,#23862,
#23863,#23864,#23865,#23866,#23867,#23868,#23869,#23870,#23871,#23872,#23873,
#23874,#23875,#23876,#23877,#23878,#23879,#23880,#23881,#23882,#23883,#23884,
#23885,#23886,#23887,#23888,#23889,#23890,#23891,#23892,#23893,#23894,#23895,
#23896,#23897,#23898,#23899,#23900,#23901,#23902,#23903,#23904,#23905,#23906,
#23907,#23908,#23909,#23910));
#24940=CLOSED_SHELL('',(#23911,#23912,#23913,#23914,#23915,#23916,#23917,
#23918,#23919,#23920,#23921,#23922,#23923,#23924,#23925,#23926,#23927,#23928,
#23929,#23930,#23931,#23932,#23933,#23934,#23935,#23936,#23937,#23938,#23939,
#23940,#23941,#23942,#23943,#23944,#23945,#23946,#23947,#23948,#23949,#23950,
#23951,#23952,#23953,#23954,#23955,#23956,#23957,#23958,#23959,#23960,#23961,
#23962,#23963,#23964,#23965,#23966,#23967,#23968,#23969,#23970,#23971,#23972,
#23973,#23974,#23975,#23976,#23977,#23978,#23979,#23980,#23981,#23982,#23983,
#23984,#23985,#23986,#23987,#23988,#23989,#23990,#23991,#23992,#23993,#23994,
#23995,#23996,#23997,#23998,#23999,#24000,#24001,#24002,#24003,#24004,#24005,
#24006,#24007,#24008,#24009,#24010,#24011,#24012,#24013,#24014,#24015,#24016,
#24017,#24018,#24019,#24020,#24021,#24022,#24023,#24024,#24025,#24026,#24027,
#24028,#24029,#24030,#24031,#24032,#24033,#24034,#24035,#24036,#24037,#24038,
#24039,#24040,#24041,#24042,#24043,#24044,#24045,#24046,#24047,#24048,#24049,
#24050,#24051,#24052,#24053,#24054,#24055,#24056,#24057,#24058,#24059,#24060,
#24061,#24062,#24063,#24064,#24065,#24066,#24067,#24068,#24069,#24070,#24071,
#24072,#24073,#24074,#24075,#24076,#24077,#24078,#24079,#24080,#24081,#24082,
#24083,#24084,#24085,#24086,#24087,#24088,#24089,#24090,#24091,#24092,#24093,
#24094,#24095,#24096,#24097,#24098,#24099,#24100,#24101,#24102,#24103,#24104,
#24105,#24106,#24107,#24108,#24109,#24110,#24111,#24112,#24113,#24114,#24115,
#24116,#24117,#24118,#24119,#24120,#24121,#24122,#24123,#24124,#24125,#24126,
#24127,#24128,#24129,#24130,#24131,#24132,#24133,#24134,#24135,#24136,#24137,
#24138,#24139,#24140,#24141,#24142,#24143,#24144,#24145,#24146,#24147,#24148,
#24149,#24150,#24151,#24152,#24153,#24154,#24155,#24156,#24157,#24158,#24159,
#24160,#24161,#24162,#24163,#24164,#24165,#24166,#24167,#24168,#24169,#24170,
#24171,#24172,#24173,#24174,#24175,#24176,#24177,#24178,#24179,#24180,#24181,
#24182,#24183,#24184,#24185,#24186,#24187,#24188,#24189,#24190,#24191,#24192,
#24193,#24194,#24195,#24196,#24197,#24198,#24199,#24200,#24201,#24202,#24203,
#24204,#24205,#24206,#24207,#24208,#24209,#24210,#24211,#24212,#24213,#24214,
#24215,#24216,#24217,#24218,#24219,#24220,#24221,#24222,#24223,#24224,#24225,
#24226,#24227,#24228,#24229,#24230,#24231,#24232,#24233,#24234,#24235,#24236,
#24237,#24238,#24239,#24240,#24241,#24242,#24243,#24244,#24245,#24246,#24247,
#24248,#24249,#24250,#24251,#24252,#24253,#24254,#24255,#24256,#24257,#24258,
#24259,#24260));
#24941=CLOSED_SHELL('',(#24261,#24262,#24263,#24264,#24265,#24266,#24267,
#24268,#24269,#24270,#24271,#24272,#24273,#24274,#24275,#24276,#24277,#24278,
#24279,#24280,#24281,#24282,#24283,#24284,#24285,#24286,#24287,#24288,#24289,
#24290,#24291,#24292,#24293,#24294,#24295,#24296,#24297,#24298,#24299,#24300,
#24301,#24302,#24303,#24304,#24305,#24306,#24307,#24308,#24309,#24310,#24311,
#24312,#24313,#24314,#24315,#24316,#24317,#24318,#24319,#24320,#24321,#24322,
#24323,#24324,#24325,#24326,#24327,#24328,#24329,#24330,#24331,#24332,#24333,
#24334,#24335,#24336,#24337,#24338,#24339,#24340,#24341,#24342,#24343,#24344,
#24345,#24346,#24347,#24348,#24349,#24350,#24351,#24352,#24353,#24354,#24355,
#24356,#24357,#24358,#24359,#24360,#24361,#24362,#24363,#24364,#24365,#24366,
#24367,#24368,#24369,#24370,#24371,#24372,#24373,#24374,#24375,#24376,#24377,
#24378,#24379,#24380,#24381,#24382,#24383,#24384,#24385,#24386,#24387,#24388,
#24389,#24390,#24391,#24392,#24393,#24394,#24395,#24396,#24397,#24398,#24399,
#24400,#24401,#24402,#24403,#24404,#24405,#24406,#24407,#24408,#24409,#24410,
#24411,#24412,#24413,#24414,#24415,#24416,#24417,#24418,#24419,#24420,#24421,
#24422,#24423,#24424,#24425,#24426,#24427,#24428,#24429,#24430,#24431,#24432,
#24433,#24434,#24435,#24436,#24437,#24438,#24439,#24440,#24441,#24442,#24443,
#24444,#24445,#24446,#24447,#24448,#24449,#24450,#24451,#24452,#24453,#24454,
#24455,#24456,#24457,#24458,#24459,#24460,#24461,#24462,#24463,#24464,#24465,
#24466,#24467,#24468,#24469,#24470,#24471,#24472,#24473,#24474,#24475,#24476,
#24477,#24478,#24479,#24480,#24481,#24482,#24483,#24484,#24485,#24486,#24487,
#24488,#24489,#24490,#24491,#24492,#24493,#24494,#24495,#24496,#24497,#24498,
#24499,#24500,#24501,#24502,#24503,#24504,#24505,#24506,#24507,#24508,#24509,
#24510,#24511,#24512,#24513,#24514,#24515,#24516,#24517,#24518,#24519,#24520,
#24521,#24522,#24523,#24524,#24525,#24526,#24527,#24528,#24529,#24530,#24531,
#24532,#24533,#24534,#24535,#24536,#24537,#24538,#24539,#24540,#24541,#24542,
#24543,#24544,#24545,#24546,#24547,#24548,#24549,#24550,#24551,#24552,#24553,
#24554,#24555,#24556,#24557,#24558,#24559,#24560,#24561,#24562,#24563,#24564,
#24565,#24566,#24567,#24568,#24569,#24570,#24571,#24572,#24573,#24574,#24575,
#24576,#24577,#24578,#24579,#24580,#24581,#24582,#24583,#24584,#24585,#24586,
#24587,#24588,#24589,#24590,#24591,#24592,#24593,#24594,#24595,#24596,#24597,
#24598,#24599,#24600,#24601,#24602));
#24942=CLOSED_SHELL('',(#24603,#24604,#24605,#24606,#24607,#24608,#24609,
#24610,#24611,#24612,#24613,#24614,#24615,#24616,#24617,#24618));
#24943=CLOSED_SHELL('',(#24619,#24620,#24621,#24622,#24623,#24624,#24625,
#24626,#24627,#24628));
#24944=CLOSED_SHELL('',(#24629,#24630,#24631,#24632,#24633,#24634,#24635,
#24636,#24637,#24638,#24639,#24640,#24641,#24642,#24643,#24644,#24645,#24646));
#24945=CLOSED_SHELL('',(#24647,#24648,#24649,#24650,#24651,#24652,#24653,
#24654,#24655,#24656,#24657,#24658,#24659,#24660,#24661,#24662,#24663,#24664));
#24946=CLOSED_SHELL('',(#24665,#24666,#24667,#24668));
#24947=CLOSED_SHELL('',(#24669,#24670,#24671,#24672,#24673,#24674,#24675,
#24676,#24677,#24678,#24679,#24680,#24681,#24682,#24683,#24684,#24685,#24686,
#24687,#24688,#24689,#24690,#24691,#24692,#24693,#24694,#24695,#24696,#24697,
#24698,#24699,#24700,#24701,#24702,#24703,#24704,#24705,#24706,#24707,#24708,
#24709,#24710,#24711,#24712,#24713));
#24948=CLOSED_SHELL('',(#24714,#24715,#24716,#24717,#24718,#24719,#24720,
#24721,#24722,#24723,#24724,#24725));
#24949=CLOSED_SHELL('',(#24726,#24727,#24728,#24729,#24730,#24731,#24732,
#24733,#24734,#24735,#24736,#24737,#24738,#24739,#24740,#24741,#24742,#24743,
#24744,#24745,#24746,#24747,#24748,#24749,#24750,#24751,#24752,#24753,#24754,
#24755,#24756,#24757,#24758,#24759,#24760,#24761,#24762,#24763,#24764,#24765,
#24766,#24767,#24768,#24769,#24770,#24771,#24772,#24773,#24774,#24775,#24776,
#24777,#24778,#24779,#24780,#24781,#24782,#24783,#24784,#24785,#24786,#24787,
#24788,#24789,#24790,#24791,#24792,#24793,#24794,#24795,#24796,#24797,#24798,
#24799,#24800,#24801,#24802,#24803,#24804,#24805,#24806,#24807,#24808,#24809,
#24810,#24811,#24812,#24813,#24814,#24815,#24816,#24817,#24818,#24819,#24820,
#24821,#24822,#24823,#24824,#24825,#24826,#24827,#24828,#24829,#24830,#24831,
#24832,#24833,#24834,#24835,#24836,#24837,#24838,#24839,#24840,#24841,#24842,
#24843,#24844,#24845,#24846,#24847,#24848,#24849,#24850,#24851,#24852,#24853,
#24854,#24855,#24856,#24857,#24858,#24859,#24860,#24861,#24862,#24863,#24864,
#24865,#24866,#24867,#24868,#24869,#24870,#24871,#24872,#24873,#24874,#24875,
#24876,#24877,#24878,#24879,#24880,#24881,#24882,#24883,#24884,#24885,#24886,
#24887,#24888,#24889,#24890,#24891,#24892,#24893,#24894,#24895,#24896,#24897,
#24898,#24899,#24900,#24901,#24902,#24903,#24904,#24905,#24906,#24907,#24908,
#24909,#24910,#24911,#24912,#24913,#24914,#24915,#24916,#24917,#24918,#24919,
#24920,#24921,#24922,#24923,#24924,#24925,#24926,#24927,#24928,#24929,#24930,
#24931));
#24950=CLOSED_SHELL('',(#24932,#24933,#24934,#24935,#24936));
#24951=DERIVED_UNIT_ELEMENT(#24979,1.);
#24952=DERIVED_UNIT_ELEMENT(#46397,-3.);
#24953=DERIVED_UNIT_ELEMENT(#24979,1.);
#24954=DERIVED_UNIT_ELEMENT(#46397,-3.);
#24955=DERIVED_UNIT_ELEMENT(#24979,1.);
#24956=DERIVED_UNIT_ELEMENT(#46397,-3.);
#24957=DERIVED_UNIT_ELEMENT(#24979,1.);
#24958=DERIVED_UNIT_ELEMENT(#46397,-3.);
#24959=DERIVED_UNIT_ELEMENT(#24979,1.);
#24960=DERIVED_UNIT_ELEMENT(#46397,-3.);
#24961=DERIVED_UNIT_ELEMENT(#24979,1.);
#24962=DERIVED_UNIT_ELEMENT(#46397,-3.);
#24963=DERIVED_UNIT_ELEMENT(#24979,1.);
#24964=DERIVED_UNIT_ELEMENT(#46397,-3.);
#24965=DERIVED_UNIT_ELEMENT(#24979,1.);
#24966=DERIVED_UNIT_ELEMENT(#46397,-3.);
#24967=DERIVED_UNIT_ELEMENT(#24979,1.);
#24968=DERIVED_UNIT_ELEMENT(#46397,-3.);
#24969=DERIVED_UNIT_ELEMENT(#24979,1.);
#24970=DERIVED_UNIT_ELEMENT(#46397,-3.);
#24971=DERIVED_UNIT_ELEMENT(#24979,1.);
#24972=DERIVED_UNIT_ELEMENT(#46397,-3.);
#24973=DERIVED_UNIT_ELEMENT(#24979,1.);
#24974=DERIVED_UNIT_ELEMENT(#46397,-3.);
#24975=DERIVED_UNIT_ELEMENT(#24979,1.);
#24976=DERIVED_UNIT_ELEMENT(#46397,-3.);
#24977=DERIVED_UNIT_ELEMENT(#24979,1.);
#24978=DERIVED_UNIT_ELEMENT(#46397,-3.);
#24979=(
MASS_UNIT()
NAMED_UNIT(*)
SI_UNIT(.KILO.,.GRAM.)
);
#24980=DERIVED_UNIT((#24951,#24952));
#24981=DERIVED_UNIT((#24953,#24954));
#24982=DERIVED_UNIT((#24955,#24956));
#24983=DERIVED_UNIT((#24957,#24958));
#24984=DERIVED_UNIT((#24959,#24960));
#24985=DERIVED_UNIT((#24961,#24962));
#24986=DERIVED_UNIT((#24963,#24964));
#24987=DERIVED_UNIT((#24965,#24966));
#24988=DERIVED_UNIT((#24967,#24968));
#24989=DERIVED_UNIT((#24969,#24970));
#24990=DERIVED_UNIT((#24971,#24972));
#24991=DERIVED_UNIT((#24973,#24974));
#24992=DERIVED_UNIT((#24975,#24976));
#24993=DERIVED_UNIT((#24977,#24978));
#24994=MEASURE_REPRESENTATION_ITEM('density measure',
POSITIVE_RATIO_MEASURE(7850.),#24980);
#24995=MEASURE_REPRESENTATION_ITEM('density measure',
POSITIVE_RATIO_MEASURE(7850.),#24981);
#24996=MEASURE_REPRESENTATION_ITEM('density measure',
POSITIVE_RATIO_MEASURE(7850.),#24982);
#24997=MEASURE_REPRESENTATION_ITEM('density measure',
POSITIVE_RATIO_MEASURE(7850.),#24983);
#24998=MEASURE_REPRESENTATION_ITEM('density measure',
POSITIVE_RATIO_MEASURE(7850.),#24984);
#24999=MEASURE_REPRESENTATION_ITEM('density measure',
POSITIVE_RATIO_MEASURE(7850.),#24985);
#25000=MEASURE_REPRESENTATION_ITEM('density measure',
POSITIVE_RATIO_MEASURE(7850.),#24986);
#25001=MEASURE_REPRESENTATION_ITEM('density measure',
POSITIVE_RATIO_MEASURE(7850.),#24987);
#25002=MEASURE_REPRESENTATION_ITEM('density measure',
POSITIVE_RATIO_MEASURE(7850.),#24988);
#25003=MEASURE_REPRESENTATION_ITEM('density measure',
POSITIVE_RATIO_MEASURE(7850.),#24989);
#25004=MEASURE_REPRESENTATION_ITEM('density measure',
POSITIVE_RATIO_MEASURE(7850.),#24990);
#25005=MEASURE_REPRESENTATION_ITEM('density measure',
POSITIVE_RATIO_MEASURE(7850.),#24991);
#25006=MEASURE_REPRESENTATION_ITEM('density measure',
POSITIVE_RATIO_MEASURE(7850.),#24992);
#25007=MEASURE_REPRESENTATION_ITEM('density measure',
POSITIVE_RATIO_MEASURE(7850.),#24993);
#25008=PROPERTY_DEFINITION_REPRESENTATION(#25078,#25036);
#25009=PROPERTY_DEFINITION_REPRESENTATION(#25079,#25037);
#25010=PROPERTY_DEFINITION_REPRESENTATION(#25080,#25038);
#25011=PROPERTY_DEFINITION_REPRESENTATION(#25081,#25039);
#25012=PROPERTY_DEFINITION_REPRESENTATION(#25082,#25040);
#25013=PROPERTY_DEFINITION_REPRESENTATION(#25083,#25041);
#25014=PROPERTY_DEFINITION_REPRESENTATION(#25084,#25042);
#25015=PROPERTY_DEFINITION_REPRESENTATION(#25085,#25043);
#25016=PROPERTY_DEFINITION_REPRESENTATION(#25086,#25044);
#25017=PROPERTY_DEFINITION_REPRESENTATION(#25087,#25045);
#25018=PROPERTY_DEFINITION_REPRESENTATION(#25088,#25046);
#25019=PROPERTY_DEFINITION_REPRESENTATION(#25089,#25047);
#25020=PROPERTY_DEFINITION_REPRESENTATION(#25090,#25048);
#25021=PROPERTY_DEFINITION_REPRESENTATION(#25091,#25049);
#25022=PROPERTY_DEFINITION_REPRESENTATION(#25092,#25050);
#25023=PROPERTY_DEFINITION_REPRESENTATION(#25093,#25051);
#25024=PROPERTY_DEFINITION_REPRESENTATION(#25094,#25052);
#25025=PROPERTY_DEFINITION_REPRESENTATION(#25095,#25053);
#25026=PROPERTY_DEFINITION_REPRESENTATION(#25096,#25054);
#25027=PROPERTY_DEFINITION_REPRESENTATION(#25097,#25055);
#25028=PROPERTY_DEFINITION_REPRESENTATION(#25098,#25056);
#25029=PROPERTY_DEFINITION_REPRESENTATION(#25099,#25057);
#25030=PROPERTY_DEFINITION_REPRESENTATION(#25100,#25058);
#25031=PROPERTY_DEFINITION_REPRESENTATION(#25101,#25059);
#25032=PROPERTY_DEFINITION_REPRESENTATION(#25102,#25060);
#25033=PROPERTY_DEFINITION_REPRESENTATION(#25103,#25061);
#25034=PROPERTY_DEFINITION_REPRESENTATION(#25104,#25062);
#25035=PROPERTY_DEFINITION_REPRESENTATION(#25105,#25063);
#25036=REPRESENTATION('material name',(#25064),#46381);
#25037=REPRESENTATION('density',(#24994),#46381);
#25038=REPRESENTATION('material name',(#25065),#46382);
#25039=REPRESENTATION('density',(#24995),#46382);
#25040=REPRESENTATION('material name',(#25066),#46383);
#25041=REPRESENTATION('density',(#24996),#46383);
#25042=REPRESENTATION('material name',(#25067),#46384);
#25043=REPRESENTATION('density',(#24997),#46384);
#25044=REPRESENTATION('material name',(#25068),#46385);
#25045=REPRESENTATION('density',(#24998),#46385);
#25046=REPRESENTATION('material name',(#25069),#46386);
#25047=REPRESENTATION('density',(#24999),#46386);
#25048=REPRESENTATION('material name',(#25070),#46387);
#25049=REPRESENTATION('density',(#25000),#46387);
#25050=REPRESENTATION('material name',(#25071),#46388);
#25051=REPRESENTATION('density',(#25001),#46388);
#25052=REPRESENTATION('material name',(#25072),#46389);
#25053=REPRESENTATION('density',(#25002),#46389);
#25054=REPRESENTATION('material name',(#25073),#46390);
#25055=REPRESENTATION('density',(#25003),#46390);
#25056=REPRESENTATION('material name',(#25074),#46391);
#25057=REPRESENTATION('density',(#25004),#46391);
#25058=REPRESENTATION('material name',(#25075),#46392);
#25059=REPRESENTATION('density',(#25005),#46392);
#25060=REPRESENTATION('material name',(#25076),#46393);
#25061=REPRESENTATION('density',(#25006),#46393);
#25062=REPRESENTATION('material name',(#25077),#46394);
#25063=REPRESENTATION('density',(#25007),#46394);
#25064=DESCRIPTIVE_REPRESENTATION_ITEM('Steel','Steel');
#25065=DESCRIPTIVE_REPRESENTATION_ITEM('Steel','Steel');
#25066=DESCRIPTIVE_REPRESENTATION_ITEM('Steel','Steel');
#25067=DESCRIPTIVE_REPRESENTATION_ITEM('Steel','Steel');
#25068=DESCRIPTIVE_REPRESENTATION_ITEM('Steel','Steel');
#25069=DESCRIPTIVE_REPRESENTATION_ITEM('Steel','Steel');
#25070=DESCRIPTIVE_REPRESENTATION_ITEM('Steel','Steel');
#25071=DESCRIPTIVE_REPRESENTATION_ITEM('Steel','Steel');
#25072=DESCRIPTIVE_REPRESENTATION_ITEM('Steel','Steel');
#25073=DESCRIPTIVE_REPRESENTATION_ITEM('Steel','Steel');
#25074=DESCRIPTIVE_REPRESENTATION_ITEM('Steel','Steel');
#25075=DESCRIPTIVE_REPRESENTATION_ITEM('Steel','Steel');
#25076=DESCRIPTIVE_REPRESENTATION_ITEM('Steel','Steel');
#25077=DESCRIPTIVE_REPRESENTATION_ITEM('Steel','Steel');
#25078=PROPERTY_DEFINITION('material property','material name',#46472);
#25079=PROPERTY_DEFINITION('material property','density of part',#46472);
#25080=PROPERTY_DEFINITION('material property','material name',#46473);
#25081=PROPERTY_DEFINITION('material property','density of part',#46473);
#25082=PROPERTY_DEFINITION('material property','material name',#46474);
#25083=PROPERTY_DEFINITION('material property','density of part',#46474);
#25084=PROPERTY_DEFINITION('material property','material name',#46475);
#25085=PROPERTY_DEFINITION('material property','density of part',#46475);
#25086=PROPERTY_DEFINITION('material property','material name',#46476);
#25087=PROPERTY_DEFINITION('material property','density of part',#46476);
#25088=PROPERTY_DEFINITION('material property','material name',#46477);
#25089=PROPERTY_DEFINITION('material property','density of part',#46477);
#25090=PROPERTY_DEFINITION('material property','material name',#46478);
#25091=PROPERTY_DEFINITION('material property','density of part',#46478);
#25092=PROPERTY_DEFINITION('material property','material name',#46479);
#25093=PROPERTY_DEFINITION('material property','density of part',#46479);
#25094=PROPERTY_DEFINITION('material property','material name',#46480);
#25095=PROPERTY_DEFINITION('material property','density of part',#46480);
#25096=PROPERTY_DEFINITION('material property','material name',#46481);
#25097=PROPERTY_DEFINITION('material property','density of part',#46481);
#25098=PROPERTY_DEFINITION('material property','material name',#46482);
#25099=PROPERTY_DEFINITION('material property','density of part',#46482);
#25100=PROPERTY_DEFINITION('material property','material name',#46483);
#25101=PROPERTY_DEFINITION('material property','density of part',#46483);
#25102=PROPERTY_DEFINITION('material property','material name',#46484);
#25103=PROPERTY_DEFINITION('material property','density of part',#46484);
#25104=PROPERTY_DEFINITION('material property','material name',#46485);
#25105=PROPERTY_DEFINITION('material property','density of part',#46485);
#25106=AXIS2_PLACEMENT_3D('',#33456,#26933,#26934);
#25107=AXIS2_PLACEMENT_3D('',#33457,#26935,#26936);
#25108=AXIS2_PLACEMENT_3D('',#33458,#26937,#26938);
#25109=AXIS2_PLACEMENT_3D('',#33460,#26939,#26940);
#25110=AXIS2_PLACEMENT_3D('',#33463,#26942,#26943);
#25111=AXIS2_PLACEMENT_3D('',#33464,#26944,#26945);
#25112=AXIS2_PLACEMENT_3D('',#33466,#26946,#26947);
#25113=AXIS2_PLACEMENT_3D('',#33467,#26948,#26949);
#25114=AXIS2_PLACEMENT_3D('',#33470,#26951,#26952);
#25115=AXIS2_PLACEMENT_3D('',#33471,#26953,#26954);
#25116=AXIS2_PLACEMENT_3D('',#33473,#26955,#26956);
#25117=AXIS2_PLACEMENT_3D('',#33476,#26958,#26959);
#25118=AXIS2_PLACEMENT_3D('',#33477,#26960,#26961);
#25119=AXIS2_PLACEMENT_3D('',#33479,#26962,#26963);
#25120=AXIS2_PLACEMENT_3D('',#33480,#26964,#26965);
#25121=AXIS2_PLACEMENT_3D('',#33483,#26967,#26968);
#25122=AXIS2_PLACEMENT_3D('',#33484,#26969,#26970);
#25123=AXIS2_PLACEMENT_3D('',#33486,#26971,#26972);
#25124=AXIS2_PLACEMENT_3D('',#33490,#26974,#26975);
#25125=AXIS2_PLACEMENT_3D('',#33491,#26976,#26977);
#25126=AXIS2_PLACEMENT_3D('',#33492,#26978,#26979);
#25127=AXIS2_PLACEMENT_3D('',#33495,#26981,#26982);
#25128=AXIS2_PLACEMENT_3D('',#33496,#26983,#26984);
#25129=AXIS2_PLACEMENT_3D('',#33498,#26985,#26986);
#25130=AXIS2_PLACEMENT_3D('',#33499,#26987,#26988);
#25131=AXIS2_PLACEMENT_3D('',#33501,#26989,#26990);
#25132=AXIS2_PLACEMENT_3D('',#33503,#26992,#26993);
#25133=AXIS2_PLACEMENT_3D('',#33508,#26995,#26996);
#25134=AXIS2_PLACEMENT_3D('',#33511,#26998,#26999);
#25135=AXIS2_PLACEMENT_3D('',#33694,#27002,#27003);
#25136=AXIS2_PLACEMENT_3D('',#33700,#27007,#27008);
#25137=AXIS2_PLACEMENT_3D('',#33705,#27010,#27011);
#25138=AXIS2_PLACEMENT_3D('',#33709,#27013,#27014);
#25139=AXIS2_PLACEMENT_3D('',#33713,#27016,#27017);
#25140=AXIS2_PLACEMENT_3D('',#33717,#27019,#27020);
#25141=AXIS2_PLACEMENT_3D('',#33720,#27022,#27023);
#25142=AXIS2_PLACEMENT_3D('',#33722,#27024,#27025);
#25143=AXIS2_PLACEMENT_3D('',#33730,#27029,#27030);
#25144=AXIS2_PLACEMENT_3D('',#33738,#27034,#27035);
#25145=AXIS2_PLACEMENT_3D('',#33740,#27036,#27037);
#25146=AXIS2_PLACEMENT_3D('',#33744,#27039,#27040);
#25147=AXIS2_PLACEMENT_3D('',#33748,#27042,#27043);
#25148=AXIS2_PLACEMENT_3D('',#33752,#27045,#27046);
#25149=AXIS2_PLACEMENT_3D('',#33754,#27047,#27048);
#25150=AXIS2_PLACEMENT_3D('',#33766,#27054,#27055);
#25151=AXIS2_PLACEMENT_3D('',#33770,#27057,#27058);
#25152=AXIS2_PLACEMENT_3D('',#33774,#27060,#27061);
#25153=AXIS2_PLACEMENT_3D('',#33776,#27062,#27063);
#25154=AXIS2_PLACEMENT_3D('',#33780,#27065,#27066);
#25155=AXIS2_PLACEMENT_3D('',#33782,#27067,#27068);
#25156=AXIS2_PLACEMENT_3D('',#33784,#27069,#27070);
#25157=AXIS2_PLACEMENT_3D('',#33786,#27071,#27072);
#25158=AXIS2_PLACEMENT_3D('',#33787,#27073,#27074);
#25159=AXIS2_PLACEMENT_3D('',#33790,#27075,#27076);
#25160=AXIS2_PLACEMENT_3D('',#33794,#27078,#27079);
#25161=AXIS2_PLACEMENT_3D('',#33796,#27080,#27081);
#25162=AXIS2_PLACEMENT_3D('',#33799,#27083,#27084);
#25163=AXIS2_PLACEMENT_3D('',#33800,#27085,#27086);
#25164=AXIS2_PLACEMENT_3D('',#33866,#27088,#27089);
#25165=AXIS2_PLACEMENT_3D('',#33991,#27093,#27094);
#25166=AXIS2_PLACEMENT_3D('',#33995,#27097,#27098);
#25167=AXIS2_PLACEMENT_3D('',#34012,#27100,#27101);
#25168=AXIS2_PLACEMENT_3D('',#34016,#27104,#27105);
#25169=AXIS2_PLACEMENT_3D('',#34019,#27107,#27108);
#25170=AXIS2_PLACEMENT_3D('',#34020,#27109,#27110);
#25171=AXIS2_PLACEMENT_3D('',#34022,#27111,#27112);
#25172=AXIS2_PLACEMENT_3D('',#34024,#27114,#27115);
#25173=AXIS2_PLACEMENT_3D('',#34027,#27117,#27118);
#25174=AXIS2_PLACEMENT_3D('',#34028,#27119,#27120);
#25175=AXIS2_PLACEMENT_3D('',#34030,#27121,#27122);
#25176=AXIS2_PLACEMENT_3D('',#34032,#27124,#27125);
#25177=AXIS2_PLACEMENT_3D('',#34051,#27128,#27129);
#25178=AXIS2_PLACEMENT_3D('',#34053,#27130,#27131);
#25179=AXIS2_PLACEMENT_3D('',#34057,#27133,#27134);
#25180=AXIS2_PLACEMENT_3D('',#34067,#27135,#27136);
#25181=AXIS2_PLACEMENT_3D('',#34079,#27138,#27139);
#25182=AXIS2_PLACEMENT_3D('',#34080,#27140,#27141);
#25183=AXIS2_PLACEMENT_3D('',#34099,#27144,#27145);
#25184=AXIS2_PLACEMENT_3D('',#34101,#27146,#27147);
#25185=AXIS2_PLACEMENT_3D('',#34104,#27149,#27150);
#25186=AXIS2_PLACEMENT_3D('',#34115,#27151,#27152);
#25187=AXIS2_PLACEMENT_3D('',#34127,#27154,#27155);
#25188=AXIS2_PLACEMENT_3D('',#34128,#27156,#27157);
#25189=AXIS2_PLACEMENT_3D('',#34144,#27159,#27160);
#25190=AXIS2_PLACEMENT_3D('',#34160,#27162,#27163);
#25191=AXIS2_PLACEMENT_3D('',#34162,#27164,#27165);
#25192=AXIS2_PLACEMENT_3D('',#34164,#27167,#27168);
#25193=AXIS2_PLACEMENT_3D('',#34167,#27169,#27170);
#25194=AXIS2_PLACEMENT_3D('',#34171,#27172,#27173);
#25195=AXIS2_PLACEMENT_3D('',#34175,#27175,#27176);
#25196=AXIS2_PLACEMENT_3D('',#34179,#27178,#27179);
#25197=AXIS2_PLACEMENT_3D('',#34182,#27181,#27182);
#25198=AXIS2_PLACEMENT_3D('',#34184,#27183,#27184);
#25199=AXIS2_PLACEMENT_3D('',#34186,#27185,#27186);
#25200=AXIS2_PLACEMENT_3D('',#34191,#27188,#27189);
#25201=AXIS2_PLACEMENT_3D('',#34194,#27191,#27192);
#25202=AXIS2_PLACEMENT_3D('',#34196,#27193,#27194);
#25203=AXIS2_PLACEMENT_3D('',#34198,#27195,#27196);
#25204=AXIS2_PLACEMENT_3D('',#34200,#27197,#27198);
#25205=AXIS2_PLACEMENT_3D('',#34202,#27199,#27200);
#25206=AXIS2_PLACEMENT_3D('',#34203,#27201,#27202);
#25207=AXIS2_PLACEMENT_3D('',#34205,#27204,#27205);
#25208=AXIS2_PLACEMENT_3D('',#34207,#27207,#27208);
#25209=AXIS2_PLACEMENT_3D('',#34209,#27210,#27211);
#25210=AXIS2_PLACEMENT_3D('',#34212,#27213,#27214);
#25211=AXIS2_PLACEMENT_3D('',#34213,#27215,#27216);
#25212=AXIS2_PLACEMENT_3D('',#34215,#27217,#27218);
#25213=AXIS2_PLACEMENT_3D('',#34217,#27220,#27221);
#25214=AXIS2_PLACEMENT_3D('',#34220,#27223,#27224);
#25215=AXIS2_PLACEMENT_3D('',#34221,#27225,#27226);
#25216=AXIS2_PLACEMENT_3D('',#34223,#27227,#27228);
#25217=AXIS2_PLACEMENT_3D('',#34404,#27231,#27232);
#25218=AXIS2_PLACEMENT_3D('',#34410,#27236,#27237);
#25219=AXIS2_PLACEMENT_3D('',#34475,#27239,#27240);
#25220=AXIS2_PLACEMENT_3D('',#34595,#27244,#27245);
#25221=AXIS2_PLACEMENT_3D('',#34599,#27248,#27249);
#25222=AXIS2_PLACEMENT_3D('',#34616,#27251,#27252);
#25223=AXIS2_PLACEMENT_3D('',#34620,#27255,#27256);
#25224=AXIS2_PLACEMENT_3D('',#34622,#27258,#27259);
#25225=AXIS2_PLACEMENT_3D('',#34624,#27261,#27262);
#25226=AXIS2_PLACEMENT_3D('',#34633,#27267,#27268);
#25227=AXIS2_PLACEMENT_3D('',#34636,#27270,#27271);
#25228=AXIS2_PLACEMENT_3D('',#34637,#27272,#27273);
#25229=AXIS2_PLACEMENT_3D('',#34638,#27274,#27275);
#25230=AXIS2_PLACEMENT_3D('',#34642,#27278,#27279);
#25231=AXIS2_PLACEMENT_3D('',#34646,#27281,#27282);
#25232=AXIS2_PLACEMENT_3D('',#34647,#27283,#27284);
#25233=AXIS2_PLACEMENT_3D('',#34648,#27285,#27286);
#25234=AXIS2_PLACEMENT_3D('',#34654,#27290,#27291);
#25235=AXIS2_PLACEMENT_3D('',#34656,#27293,#27294);
#25236=AXIS2_PLACEMENT_3D('',#34672,#27295,#27296);
#25237=AXIS2_PLACEMENT_3D('',#34686,#27297,#27298);
#25238=AXIS2_PLACEMENT_3D('',#34687,#27299,#27300);
#25239=AXIS2_PLACEMENT_3D('',#34691,#27302,#27303);
#25240=AXIS2_PLACEMENT_3D('',#34693,#27305,#27306);
#25241=AXIS2_PLACEMENT_3D('',#34710,#27307,#27308);
#25242=AXIS2_PLACEMENT_3D('',#34725,#27309,#27310);
#25243=AXIS2_PLACEMENT_3D('',#34741,#27311,#27312);
#25244=AXIS2_PLACEMENT_3D('',#34742,#27313,#27314);
#25245=AXIS2_PLACEMENT_3D('',#34744,#27315,#27316);
#25246=AXIS2_PLACEMENT_3D('',#34746,#27317,#27318);
#25247=AXIS2_PLACEMENT_3D('',#34747,#27319,#27320);
#25248=AXIS2_PLACEMENT_3D('',#34748,#27321,#27322);
#25249=AXIS2_PLACEMENT_3D('',#34750,#27324,#27325);
#25250=AXIS2_PLACEMENT_3D('',#34752,#27327,#27328);
#25251=AXIS2_PLACEMENT_3D('',#34756,#27330,#27331);
#25252=AXIS2_PLACEMENT_3D('',#34758,#27333,#27334);
#25253=AXIS2_PLACEMENT_3D('',#34762,#27337,#27338);
#25254=AXIS2_PLACEMENT_3D('',#34765,#27340,#27341);
#25255=AXIS2_PLACEMENT_3D('',#34766,#27342,#27343);
#25256=AXIS2_PLACEMENT_3D('',#34783,#27344,#27345);
#25257=AXIS2_PLACEMENT_3D('',#34798,#27346,#27347);
#25258=AXIS2_PLACEMENT_3D('',#34814,#27348,#27349);
#25259=AXIS2_PLACEMENT_3D('',#34815,#27350,#27351);
#25260=AXIS2_PLACEMENT_3D('',#34817,#27352,#27353);
#25261=AXIS2_PLACEMENT_3D('',#34819,#27354,#27355);
#25262=AXIS2_PLACEMENT_3D('',#34820,#27356,#27357);
#25263=AXIS2_PLACEMENT_3D('',#34821,#27358,#27359);
#25264=AXIS2_PLACEMENT_3D('',#34823,#27361,#27362);
#25265=AXIS2_PLACEMENT_3D('',#34825,#27364,#27365);
#25266=AXIS2_PLACEMENT_3D('',#34829,#27367,#27368);
#25267=AXIS2_PLACEMENT_3D('',#34831,#27370,#27371);
#25268=AXIS2_PLACEMENT_3D('',#34835,#27374,#27375);
#25269=AXIS2_PLACEMENT_3D('',#34838,#27377,#27378);
#25270=AXIS2_PLACEMENT_3D('',#34839,#27379,#27380);
#25271=AXIS2_PLACEMENT_3D('',#34868,#27381,#27382);
#25272=AXIS2_PLACEMENT_3D('',#34870,#27383,#27384);
#25273=AXIS2_PLACEMENT_3D('',#34885,#27385,#27386);
#25274=AXIS2_PLACEMENT_3D('',#34887,#27387,#27388);
#25275=AXIS2_PLACEMENT_3D('',#34889,#27390,#27391);
#25276=AXIS2_PLACEMENT_3D('',#34906,#27392,#27393);
#25277=AXIS2_PLACEMENT_3D('',#34921,#27394,#27395);
#25278=AXIS2_PLACEMENT_3D('',#34925,#27397,#27398);
#25279=AXIS2_PLACEMENT_3D('',#34927,#27400,#27401);
#25280=AXIS2_PLACEMENT_3D('',#34931,#27403,#27404);
#25281=AXIS2_PLACEMENT_3D('',#34946,#27405,#27406);
#25282=AXIS2_PLACEMENT_3D('',#34962,#27407,#27408);
#25283=AXIS2_PLACEMENT_3D('',#34963,#27409,#27410);
#25284=AXIS2_PLACEMENT_3D('',#34979,#27411,#27412);
#25285=AXIS2_PLACEMENT_3D('',#34980,#27413,#27414);
#25286=AXIS2_PLACEMENT_3D('',#34982,#27415,#27416);
#25287=AXIS2_PLACEMENT_3D('',#34983,#27417,#27418);
#25288=AXIS2_PLACEMENT_3D('',#34984,#27419,#27420);
#25289=AXIS2_PLACEMENT_3D('',#34986,#27421,#27422);
#25290=AXIS2_PLACEMENT_3D('',#34988,#27424,#27425);
#25291=AXIS2_PLACEMENT_3D('',#34990,#27426,#27427);
#25292=AXIS2_PLACEMENT_3D('',#34991,#27428,#27429);
#25293=AXIS2_PLACEMENT_3D('',#34992,#27430,#27431);
#25294=AXIS2_PLACEMENT_3D('',#34994,#27433,#27434);
#25295=AXIS2_PLACEMENT_3D('',#34998,#27437,#27438);
#25296=AXIS2_PLACEMENT_3D('',#35001,#27440,#27441);
#25297=AXIS2_PLACEMENT_3D('',#35002,#27442,#27443);
#25298=AXIS2_PLACEMENT_3D('',#35006,#27446,#27447);
#25299=AXIS2_PLACEMENT_3D('',#35009,#27449,#27450);
#25300=AXIS2_PLACEMENT_3D('',#35010,#27451,#27452);
#25301=AXIS2_PLACEMENT_3D('',#35014,#27455,#27456);
#25302=AXIS2_PLACEMENT_3D('',#35017,#27458,#27459);
#25303=AXIS2_PLACEMENT_3D('',#35018,#27460,#27461);
#25304=AXIS2_PLACEMENT_3D('',#35021,#27463,#27464);
#25305=AXIS2_PLACEMENT_3D('',#35022,#27465,#27466);
#25306=AXIS2_PLACEMENT_3D('',#35024,#27467,#27468);
#25307=AXIS2_PLACEMENT_3D('',#35027,#27470,#27471);
#25308=AXIS2_PLACEMENT_3D('',#35028,#27472,#27473);
#25309=AXIS2_PLACEMENT_3D('',#35030,#27474,#27475);
#25310=AXIS2_PLACEMENT_3D('',#35031,#27476,#27477);
#25311=AXIS2_PLACEMENT_3D('',#35032,#27478,#27479);
#25312=AXIS2_PLACEMENT_3D('',#35034,#27480,#27481);
#25313=AXIS2_PLACEMENT_3D('',#35036,#27483,#27484);
#25314=AXIS2_PLACEMENT_3D('',#35038,#27485,#27486);
#25315=AXIS2_PLACEMENT_3D('',#35039,#27487,#27488);
#25316=AXIS2_PLACEMENT_3D('',#35040,#27489,#27490);
#25317=AXIS2_PLACEMENT_3D('',#35042,#27491,#27492);
#25318=AXIS2_PLACEMENT_3D('',#35044,#27494,#27495);
#25319=AXIS2_PLACEMENT_3D('',#35046,#27496,#27497);
#25320=AXIS2_PLACEMENT_3D('',#35047,#27498,#27499);
#25321=AXIS2_PLACEMENT_3D('',#35048,#27500,#27501);
#25322=AXIS2_PLACEMENT_3D('',#35050,#27503,#27504);
#25323=AXIS2_PLACEMENT_3D('',#35052,#27505,#27506);
#25324=AXIS2_PLACEMENT_3D('',#35053,#27507,#27508);
#25325=AXIS2_PLACEMENT_3D('',#35054,#27509,#27510);
#25326=AXIS2_PLACEMENT_3D('',#35056,#27512,#27513);
#25327=AXIS2_PLACEMENT_3D('',#35060,#27515,#27516);
#25328=AXIS2_PLACEMENT_3D('',#35062,#27518,#27519);
#25329=AXIS2_PLACEMENT_3D('',#35066,#27522,#27523);
#25330=AXIS2_PLACEMENT_3D('',#35069,#27525,#27526);
#25331=AXIS2_PLACEMENT_3D('',#35070,#27527,#27528);
#25332=AXIS2_PLACEMENT_3D('',#35074,#27531,#27532);
#25333=AXIS2_PLACEMENT_3D('',#35077,#27534,#27535);
#25334=AXIS2_PLACEMENT_3D('',#35078,#27536,#27537);
#25335=AXIS2_PLACEMENT_3D('',#35080,#27539,#27540);
#25336=AXIS2_PLACEMENT_3D('',#35082,#27542,#27543);
#25337=AXIS2_PLACEMENT_3D('',#35084,#27545,#27546);
#25338=AXIS2_PLACEMENT_3D('',#35086,#27548,#27549);
#25339=AXIS2_PLACEMENT_3D('',#35088,#27550,#27551);
#25340=AXIS2_PLACEMENT_3D('',#35103,#27552,#27553);
#25341=AXIS2_PLACEMENT_3D('',#35120,#27555,#27556);
#25342=AXIS2_PLACEMENT_3D('',#35121,#27557,#27558);
#25343=AXIS2_PLACEMENT_3D('',#35122,#27559,#27560);
#25344=AXIS2_PLACEMENT_3D('',#35124,#27561,#27562);
#25345=AXIS2_PLACEMENT_3D('',#35126,#27564,#27565);
#25346=AXIS2_PLACEMENT_3D('',#35130,#27568,#27569);
#25347=AXIS2_PLACEMENT_3D('',#35131,#27570,#27571);
#25348=AXIS2_PLACEMENT_3D('',#35132,#27572,#27573);
#25349=AXIS2_PLACEMENT_3D('',#35133,#27574,#27575);
#25350=AXIS2_PLACEMENT_3D('',#35134,#27576,#27577);
#25351=AXIS2_PLACEMENT_3D('',#35135,#27578,#27579);
#25352=AXIS2_PLACEMENT_3D('',#35136,#27580,#27581);
#25353=AXIS2_PLACEMENT_3D('',#35137,#27582,#27583);
#25354=AXIS2_PLACEMENT_3D('',#35138,#27584,#27585);
#25355=AXIS2_PLACEMENT_3D('',#35139,#27586,#27587);
#25356=AXIS2_PLACEMENT_3D('',#35140,#27588,#27589);
#25357=AXIS2_PLACEMENT_3D('',#35141,#27590,#27591);
#25358=AXIS2_PLACEMENT_3D('',#35142,#27592,#27593);
#25359=AXIS2_PLACEMENT_3D('',#35143,#27594,#27595);
#25360=AXIS2_PLACEMENT_3D('',#35145,#27596,#27597);
#25361=AXIS2_PLACEMENT_3D('',#35147,#27599,#27600);
#25362=AXIS2_PLACEMENT_3D('',#35149,#27601,#27602);
#25363=AXIS2_PLACEMENT_3D('',#35150,#27603,#27604);
#25364=AXIS2_PLACEMENT_3D('',#35151,#27605,#27606);
#25365=AXIS2_PLACEMENT_3D('',#35153,#27608,#27609);
#25366=AXIS2_PLACEMENT_3D('',#35155,#27610,#27611);
#25367=AXIS2_PLACEMENT_3D('',#35157,#27612,#27613);
#25368=AXIS2_PLACEMENT_3D('',#35158,#27614,#27615);
#25369=AXIS2_PLACEMENT_3D('',#35159,#27616,#27617);
#25370=AXIS2_PLACEMENT_3D('',#35160,#27618,#27619);
#25371=AXIS2_PLACEMENT_3D('',#35175,#27620,#27621);
#25372=AXIS2_PLACEMENT_3D('',#35191,#27623,#27624);
#25373=AXIS2_PLACEMENT_3D('',#35193,#27625,#27626);
#25374=AXIS2_PLACEMENT_3D('',#35194,#27627,#27628);
#25375=AXIS2_PLACEMENT_3D('',#35196,#27630,#27631);
#25376=AXIS2_PLACEMENT_3D('',#35198,#27633,#27634);
#25377=AXIS2_PLACEMENT_3D('',#35199,#27635,#27636);
#25378=AXIS2_PLACEMENT_3D('',#35200,#27637,#27638);
#25379=AXIS2_PLACEMENT_3D('',#35201,#27639,#27640);
#25380=AXIS2_PLACEMENT_3D('',#35202,#27641,#27642);
#25381=AXIS2_PLACEMENT_3D('',#35203,#27643,#27644);
#25382=AXIS2_PLACEMENT_3D('',#35204,#27645,#27646);
#25383=AXIS2_PLACEMENT_3D('',#35205,#27647,#27648);
#25384=AXIS2_PLACEMENT_3D('',#35206,#27649,#27650);
#25385=AXIS2_PLACEMENT_3D('',#35208,#27651,#27652);
#25386=AXIS2_PLACEMENT_3D('',#35211,#27654,#27655);
#25387=AXIS2_PLACEMENT_3D('',#35212,#27656,#27657);
#25388=AXIS2_PLACEMENT_3D('',#35214,#27658,#27659);
#25389=AXIS2_PLACEMENT_3D('',#35215,#27660,#27661);
#25390=AXIS2_PLACEMENT_3D('',#35216,#27662,#27663);
#25391=AXIS2_PLACEMENT_3D('',#35218,#27664,#27665);
#25392=AXIS2_PLACEMENT_3D('',#35220,#27667,#27668);
#25393=AXIS2_PLACEMENT_3D('',#35221,#27669,#27670);
#25394=AXIS2_PLACEMENT_3D('',#35222,#27671,#27672);
#25395=AXIS2_PLACEMENT_3D('',#35226,#27674,#27675);
#25396=AXIS2_PLACEMENT_3D('',#35228,#27677,#27678);
#25397=AXIS2_PLACEMENT_3D('',#35232,#27681,#27682);
#25398=AXIS2_PLACEMENT_3D('',#35234,#27683,#27684);
#25399=AXIS2_PLACEMENT_3D('',#35237,#27686,#27687);
#25400=AXIS2_PLACEMENT_3D('',#35238,#27688,#27689);
#25401=AXIS2_PLACEMENT_3D('',#35240,#27690,#27691);
#25402=AXIS2_PLACEMENT_3D('',#35241,#27692,#27693);
#25403=AXIS2_PLACEMENT_3D('',#35242,#27694,#27695);
#25404=AXIS2_PLACEMENT_3D('',#35244,#27696,#27697);
#25405=AXIS2_PLACEMENT_3D('',#35246,#27699,#27700);
#25406=AXIS2_PLACEMENT_3D('',#35247,#27701,#27702);
#25407=AXIS2_PLACEMENT_3D('',#35248,#27703,#27704);
#25408=AXIS2_PLACEMENT_3D('',#35252,#27706,#27707);
#25409=AXIS2_PLACEMENT_3D('',#35254,#27709,#27710);
#25410=AXIS2_PLACEMENT_3D('',#35258,#27713,#27714);
#25411=AXIS2_PLACEMENT_3D('',#35261,#27716,#27717);
#25412=AXIS2_PLACEMENT_3D('',#35262,#27718,#27719);
#25413=AXIS2_PLACEMENT_3D('',#35264,#27721,#27722);
#25414=AXIS2_PLACEMENT_3D('',#35267,#27724,#27725);
#25415=AXIS2_PLACEMENT_3D('',#35268,#27726,#27727);
#25416=AXIS2_PLACEMENT_3D('',#35270,#27729,#27730);
#25417=AXIS2_PLACEMENT_3D('',#35271,#27731,#27732);
#25418=AXIS2_PLACEMENT_3D('',#35274,#27734,#27735);
#25419=AXIS2_PLACEMENT_3D('',#35275,#27736,#27737);
#25420=AXIS2_PLACEMENT_3D('',#35276,#27738,#27739);
#25421=AXIS2_PLACEMENT_3D('',#35279,#27741,#27742);
#25422=AXIS2_PLACEMENT_3D('',#35280,#27743,#27744);
#25423=AXIS2_PLACEMENT_3D('',#35281,#27745,#27746);
#25424=AXIS2_PLACEMENT_3D('',#35283,#27747,#27748);
#25425=AXIS2_PLACEMENT_3D('',#35285,#27749,#27750);
#25426=AXIS2_PLACEMENT_3D('',#35286,#27751,#27752);
#25427=AXIS2_PLACEMENT_3D('',#35289,#27754,#27755);
#25428=AXIS2_PLACEMENT_3D('',#35290,#27756,#27757);
#25429=AXIS2_PLACEMENT_3D('',#35292,#27758,#27759);
#25430=AXIS2_PLACEMENT_3D('',#35293,#27760,#27761);
#25431=AXIS2_PLACEMENT_3D('',#35295,#27763,#27764);
#25432=AXIS2_PLACEMENT_3D('',#35297,#27766,#27767);
#25433=AXIS2_PLACEMENT_3D('',#35298,#27768,#27769);
#25434=AXIS2_PLACEMENT_3D('',#35300,#27770,#27771);
#25435=AXIS2_PLACEMENT_3D('',#35302,#27773,#27774);
#25436=AXIS2_PLACEMENT_3D('',#35304,#27775,#27776);
#25437=AXIS2_PLACEMENT_3D('',#35306,#27778,#27779);
#25438=AXIS2_PLACEMENT_3D('',#35308,#27781,#27782);
#25439=AXIS2_PLACEMENT_3D('',#35310,#27784,#27785);
#25440=AXIS2_PLACEMENT_3D('',#35312,#27787,#27788);
#25441=AXIS2_PLACEMENT_3D('',#35314,#27790,#27791);
#25442=AXIS2_PLACEMENT_3D('',#35315,#27792,#27793);
#25443=AXIS2_PLACEMENT_3D('',#35316,#27794,#27795);
#25444=AXIS2_PLACEMENT_3D('',#35318,#27797,#27798);
#25445=AXIS2_PLACEMENT_3D('',#35319,#27799,#27800);
#25446=AXIS2_PLACEMENT_3D('',#35320,#27801,#27802);
#25447=AXIS2_PLACEMENT_3D('',#35322,#27803,#27804);
#25448=AXIS2_PLACEMENT_3D('',#35325,#27806,#27807);
#25449=AXIS2_PLACEMENT_3D('',#35326,#27808,#27809);
#25450=AXIS2_PLACEMENT_3D('',#35329,#27811,#27812);
#25451=AXIS2_PLACEMENT_3D('',#35330,#27813,#27814);
#25452=AXIS2_PLACEMENT_3D('',#35332,#27815,#27816);
#25453=AXIS2_PLACEMENT_3D('',#35333,#27817,#27818);
#25454=AXIS2_PLACEMENT_3D('',#35335,#27819,#27820);
#25455=AXIS2_PLACEMENT_3D('',#35338,#27822,#27823);
#25456=AXIS2_PLACEMENT_3D('',#35339,#27824,#27825);
#25457=AXIS2_PLACEMENT_3D('',#35342,#27827,#27828);
#25458=AXIS2_PLACEMENT_3D('',#35343,#27829,#27830);
#25459=AXIS2_PLACEMENT_3D('',#35345,#27831,#27832);
#25460=AXIS2_PLACEMENT_3D('',#35346,#27833,#27834);
#25461=AXIS2_PLACEMENT_3D('',#35349,#27835,#27836);
#25462=AXIS2_PLACEMENT_3D('',#35353,#27838,#27839);
#25463=AXIS2_PLACEMENT_3D('',#35355,#27841,#27842);
#25464=AXIS2_PLACEMENT_3D('',#35358,#27843,#27844);
#25465=AXIS2_PLACEMENT_3D('',#35359,#27845,#27846);
#25466=AXIS2_PLACEMENT_3D('',#35360,#27847,#27848);
#25467=AXIS2_PLACEMENT_3D('',#35361,#27849,#27850);
#25468=AXIS2_PLACEMENT_3D('',#35364,#27851,#27852);
#25469=AXIS2_PLACEMENT_3D('',#35367,#27855,#27856);
#25470=AXIS2_PLACEMENT_3D('',#35370,#27857,#27858);
#25471=AXIS2_PLACEMENT_3D('',#35371,#27859,#27860);
#25472=AXIS2_PLACEMENT_3D('',#35372,#27861,#27862);
#25473=AXIS2_PLACEMENT_3D('',#35373,#27863,#27864);
#25474=AXIS2_PLACEMENT_3D('',#35376,#27865,#27866);
#25475=AXIS2_PLACEMENT_3D('',#35379,#27869,#27870);
#25476=AXIS2_PLACEMENT_3D('',#35382,#27871,#27872);
#25477=AXIS2_PLACEMENT_3D('',#35383,#27873,#27874);
#25478=AXIS2_PLACEMENT_3D('',#35384,#27875,#27876);
#25479=AXIS2_PLACEMENT_3D('',#35385,#27877,#27878);
#25480=AXIS2_PLACEMENT_3D('',#35388,#27879,#27880);
#25481=AXIS2_PLACEMENT_3D('',#35391,#27883,#27884);
#25482=AXIS2_PLACEMENT_3D('',#35392,#27885,#27886);
#25483=AXIS2_PLACEMENT_3D('',#35393,#27887,#27888);
#25484=AXIS2_PLACEMENT_3D('',#35394,#27889,#27890);
#25485=AXIS2_PLACEMENT_3D('',#35398,#27892,#27893);
#25486=AXIS2_PLACEMENT_3D('',#35400,#27895,#27896);
#25487=AXIS2_PLACEMENT_3D('',#35404,#27899,#27900);
#25488=AXIS2_PLACEMENT_3D('',#35407,#27902,#27903);
#25489=AXIS2_PLACEMENT_3D('',#35408,#27904,#27905);
#25490=AXIS2_PLACEMENT_3D('',#35413,#27908,#27909);
#25491=AXIS2_PLACEMENT_3D('',#35414,#27910,#27911);
#25492=AXIS2_PLACEMENT_3D('',#35416,#27912,#27913);
#25493=AXIS2_PLACEMENT_3D('',#35418,#27914,#27915);
#25494=AXIS2_PLACEMENT_3D('',#35421,#27916,#27917);
#25495=AXIS2_PLACEMENT_3D('',#35422,#27918,#27919);
#25496=AXIS2_PLACEMENT_3D('',#35424,#27920,#27921);
#25497=AXIS2_PLACEMENT_3D('',#35426,#27922,#27923);
#25498=AXIS2_PLACEMENT_3D('',#35428,#27924,#27925);
#25499=AXIS2_PLACEMENT_3D('',#35430,#27926,#27927);
#25500=AXIS2_PLACEMENT_3D('',#35431,#27928,#27929);
#25501=AXIS2_PLACEMENT_3D('',#35433,#27930,#27931);
#25502=AXIS2_PLACEMENT_3D('',#35435,#27932,#27933);
#25503=AXIS2_PLACEMENT_3D('',#35437,#27935,#27936);
#25504=AXIS2_PLACEMENT_3D('',#35440,#27937,#27938);
#25505=AXIS2_PLACEMENT_3D('',#35441,#27939,#27940);
#25506=AXIS2_PLACEMENT_3D('',#35442,#27941,#27942);
#25507=AXIS2_PLACEMENT_3D('',#35443,#27943,#27944);
#25508=AXIS2_PLACEMENT_3D('',#35446,#27945,#27946);
#25509=AXIS2_PLACEMENT_3D('',#35449,#27949,#27950);
#25510=AXIS2_PLACEMENT_3D('',#35452,#27951,#27952);
#25511=AXIS2_PLACEMENT_3D('',#35453,#27953,#27954);
#25512=AXIS2_PLACEMENT_3D('',#35454,#27955,#27956);
#25513=AXIS2_PLACEMENT_3D('',#35455,#27957,#27958);
#25514=AXIS2_PLACEMENT_3D('',#35457,#27959,#27960);
#25515=AXIS2_PLACEMENT_3D('',#35460,#27963,#27964);
#25516=AXIS2_PLACEMENT_3D('',#35462,#27965,#27966);
#25517=AXIS2_PLACEMENT_3D('',#35463,#27967,#27968);
#25518=AXIS2_PLACEMENT_3D('',#35464,#27969,#27970);
#25519=AXIS2_PLACEMENT_3D('',#35466,#27971,#27972);
#25520=AXIS2_PLACEMENT_3D('',#35468,#27974,#27975);
#25521=AXIS2_PLACEMENT_3D('',#35469,#27976,#27977);
#25522=AXIS2_PLACEMENT_3D('',#35470,#27978,#27979);
#25523=AXIS2_PLACEMENT_3D('',#35473,#27982,#27983);
#25524=AXIS2_PLACEMENT_3D('',#35475,#27985,#27986);
#25525=AXIS2_PLACEMENT_3D('',#35476,#27987,#27988);
#25526=AXIS2_PLACEMENT_3D('',#35478,#27989,#27990);
#25527=AXIS2_PLACEMENT_3D('',#35480,#27991,#27992);
#25528=AXIS2_PLACEMENT_3D('',#35483,#27993,#27994);
#25529=AXIS2_PLACEMENT_3D('',#35484,#27995,#27996);
#25530=AXIS2_PLACEMENT_3D('',#35486,#27997,#27998);
#25531=AXIS2_PLACEMENT_3D('',#35488,#27999,#28000);
#25532=AXIS2_PLACEMENT_3D('',#35490,#28001,#28002);
#25533=AXIS2_PLACEMENT_3D('',#35492,#28003,#28004);
#25534=AXIS2_PLACEMENT_3D('',#35493,#28005,#28006);
#25535=AXIS2_PLACEMENT_3D('',#35496,#28008,#28009);
#25536=AXIS2_PLACEMENT_3D('',#35497,#28010,#28011);
#25537=AXIS2_PLACEMENT_3D('',#35498,#28012,#28013);
#25538=AXIS2_PLACEMENT_3D('',#35501,#28015,#28016);
#25539=AXIS2_PLACEMENT_3D('',#35502,#28017,#28018);
#25540=AXIS2_PLACEMENT_3D('',#35503,#28019,#28020);
#25541=AXIS2_PLACEMENT_3D('',#35506,#28022,#28023);
#25542=AXIS2_PLACEMENT_3D('',#35507,#28024,#28025);
#25543=AXIS2_PLACEMENT_3D('',#35508,#28026,#28027);
#25544=AXIS2_PLACEMENT_3D('',#35511,#28029,#28030);
#25545=AXIS2_PLACEMENT_3D('',#35512,#28031,#28032);
#25546=AXIS2_PLACEMENT_3D('',#35513,#28033,#28034);
#25547=AXIS2_PLACEMENT_3D('',#35515,#28036,#28037);
#25548=AXIS2_PLACEMENT_3D('',#35517,#28039,#28040);
#25549=AXIS2_PLACEMENT_3D('',#35519,#28042,#28043);
#25550=AXIS2_PLACEMENT_3D('',#35521,#28045,#28046);
#25551=AXIS2_PLACEMENT_3D('',#35523,#28047,#28048);
#25552=AXIS2_PLACEMENT_3D('',#35582,#28050,#28051);
#25553=AXIS2_PLACEMENT_3D('',#35618,#28056,#28057);
#25554=AXIS2_PLACEMENT_3D('',#35619,#28058,#28059);
#25555=AXIS2_PLACEMENT_3D('',#35621,#28060,#28061);
#25556=AXIS2_PLACEMENT_3D('',#35623,#28063,#28064);
#25557=AXIS2_PLACEMENT_3D('',#35625,#28065,#28066);
#25558=AXIS2_PLACEMENT_3D('',#35653,#28068,#28069);
#25559=AXIS2_PLACEMENT_3D('',#35654,#28070,#28071);
#25560=AXIS2_PLACEMENT_3D('',#35655,#28072,#28073);
#25561=AXIS2_PLACEMENT_3D('',#35657,#28075,#28076);
#25562=AXIS2_PLACEMENT_3D('',#35658,#28077,#28078);
#25563=AXIS2_PLACEMENT_3D('',#35659,#28079,#28080);
#25564=AXIS2_PLACEMENT_3D('',#35661,#28081,#28082);
#25565=AXIS2_PLACEMENT_3D('',#35664,#28084,#28085);
#25566=AXIS2_PLACEMENT_3D('',#35665,#28086,#28087);
#25567=AXIS2_PLACEMENT_3D('',#35667,#28088,#28089);
#25568=AXIS2_PLACEMENT_3D('',#35668,#28090,#28091);
#25569=AXIS2_PLACEMENT_3D('',#35671,#28093,#28094);
#25570=AXIS2_PLACEMENT_3D('',#35672,#28095,#28096);
#25571=AXIS2_PLACEMENT_3D('',#35681,#28101,#28102);
#25572=AXIS2_PLACEMENT_3D('',#35685,#28104,#28105);
#25573=AXIS2_PLACEMENT_3D('',#35686,#28106,#28107);
#25574=AXIS2_PLACEMENT_3D('',#35687,#28108,#28109);
#25575=AXIS2_PLACEMENT_3D('',#35693,#28113,#28114);
#25576=AXIS2_PLACEMENT_3D('',#35694,#28115,#28116);
#25577=AXIS2_PLACEMENT_3D('',#35695,#28117,#28118);
#25578=AXIS2_PLACEMENT_3D('',#35696,#28119,#28120);
#25579=AXIS2_PLACEMENT_3D('',#35700,#28122,#28123);
#25580=AXIS2_PLACEMENT_3D('',#35702,#28125,#28126);
#25581=AXIS2_PLACEMENT_3D('',#35706,#28129,#28130);
#25582=AXIS2_PLACEMENT_3D('',#35709,#28131,#28132);
#25583=AXIS2_PLACEMENT_3D('',#35713,#28134,#28135);
#25584=AXIS2_PLACEMENT_3D('',#35717,#28137,#28138);
#25585=AXIS2_PLACEMENT_3D('',#35721,#28140,#28141);
#25586=AXIS2_PLACEMENT_3D('',#35724,#28143,#28144);
#25587=AXIS2_PLACEMENT_3D('',#35726,#28145,#28146);
#25588=AXIS2_PLACEMENT_3D('',#35728,#28147,#28148);
#25589=AXIS2_PLACEMENT_3D('',#35730,#28149,#28150);
#25590=AXIS2_PLACEMENT_3D('',#35732,#28151,#28152);
#25591=AXIS2_PLACEMENT_3D('',#35734,#28153,#28154);
#25592=AXIS2_PLACEMENT_3D('',#35735,#28155,#28156);
#25593=AXIS2_PLACEMENT_3D('',#35744,#28161,#28162);
#25594=AXIS2_PLACEMENT_3D('',#35748,#28164,#28165);
#25595=AXIS2_PLACEMENT_3D('',#35749,#28166,#28167);
#25596=AXIS2_PLACEMENT_3D('',#35750,#28168,#28169);
#25597=AXIS2_PLACEMENT_3D('',#35756,#28173,#28174);
#25598=AXIS2_PLACEMENT_3D('',#35757,#28175,#28176);
#25599=AXIS2_PLACEMENT_3D('',#35758,#28177,#28178);
#25600=AXIS2_PLACEMENT_3D('',#35759,#28179,#28180);
#25601=AXIS2_PLACEMENT_3D('',#35763,#28182,#28183);
#25602=AXIS2_PLACEMENT_3D('',#35765,#28185,#28186);
#25603=AXIS2_PLACEMENT_3D('',#35769,#28189,#28190);
#25604=AXIS2_PLACEMENT_3D('',#35770,#28191,#28192);
#25605=AXIS2_PLACEMENT_3D('',#35778,#28194,#28195);
#25606=AXIS2_PLACEMENT_3D('',#35783,#28196,#28197);
#25607=AXIS2_PLACEMENT_3D('',#35784,#28198,#28199);
#25608=AXIS2_PLACEMENT_3D('',#35804,#28206,#28207);
#25609=AXIS2_PLACEMENT_3D('',#35807,#28209,#28210);
#25610=AXIS2_PLACEMENT_3D('',#35808,#28211,#28212);
#25611=AXIS2_PLACEMENT_3D('',#35811,#28214,#28215);
#25612=AXIS2_PLACEMENT_3D('',#35812,#28216,#28217);
#25613=AXIS2_PLACEMENT_3D('',#35813,#28218,#28219);
#25614=AXIS2_PLACEMENT_3D('',#35816,#28221,#28222);
#25615=AXIS2_PLACEMENT_3D('',#35817,#28223,#28224);
#25616=AXIS2_PLACEMENT_3D('',#35826,#28226,#28227);
#25617=AXIS2_PLACEMENT_3D('',#35827,#28228,#28229);
#25618=AXIS2_PLACEMENT_3D('',#35832,#28230,#28231);
#25619=AXIS2_PLACEMENT_3D('',#35833,#28232,#28233);
#25620=AXIS2_PLACEMENT_3D('',#35853,#28240,#28241);
#25621=AXIS2_PLACEMENT_3D('',#35856,#28243,#28244);
#25622=AXIS2_PLACEMENT_3D('',#35857,#28245,#28246);
#25623=AXIS2_PLACEMENT_3D('',#35861,#28248,#28249);
#25624=AXIS2_PLACEMENT_3D('',#35862,#28250,#28251);
#25625=AXIS2_PLACEMENT_3D('',#35863,#28252,#28253);
#25626=AXIS2_PLACEMENT_3D('',#35864,#28254,#28255);
#25627=AXIS2_PLACEMENT_3D('',#35867,#28257,#28258);
#25628=AXIS2_PLACEMENT_3D('',#35868,#28259,#28260);
#25629=AXIS2_PLACEMENT_3D('',#35872,#28262,#28263);
#25630=AXIS2_PLACEMENT_3D('',#35874,#28265,#28266);
#25631=AXIS2_PLACEMENT_3D('',#35878,#28269,#28270);
#25632=AXIS2_PLACEMENT_3D('',#35881,#28272,#28273);
#25633=AXIS2_PLACEMENT_3D('',#35882,#28274,#28275);
#25634=AXIS2_PLACEMENT_3D('',#35886,#28278,#28279);
#25635=AXIS2_PLACEMENT_3D('',#35889,#28281,#28282);
#25636=AXIS2_PLACEMENT_3D('',#35890,#28283,#28284);
#25637=AXIS2_PLACEMENT_3D('',#35894,#28287,#28288);
#25638=AXIS2_PLACEMENT_3D('',#35897,#28290,#28291);
#25639=AXIS2_PLACEMENT_3D('',#35898,#28292,#28293);
#25640=AXIS2_PLACEMENT_3D('',#35900,#28295,#28296);
#25641=AXIS2_PLACEMENT_3D('',#35906,#28300,#28301);
#25642=AXIS2_PLACEMENT_3D('',#35909,#28303,#28304);
#25643=AXIS2_PLACEMENT_3D('',#35910,#28305,#28306);
#25644=AXIS2_PLACEMENT_3D('',#35914,#28309,#28310);
#25645=AXIS2_PLACEMENT_3D('',#35917,#28312,#28313);
#25646=AXIS2_PLACEMENT_3D('',#35918,#28314,#28315);
#25647=AXIS2_PLACEMENT_3D('',#35921,#28318,#28319);
#25648=AXIS2_PLACEMENT_3D('',#35924,#28321,#28322);
#25649=AXIS2_PLACEMENT_3D('',#35925,#28323,#28324);
#25650=AXIS2_PLACEMENT_3D('',#35929,#28327,#28328);
#25651=AXIS2_PLACEMENT_3D('',#35931,#28330,#28331);
#25652=AXIS2_PLACEMENT_3D('',#35932,#28332,#28333);
#25653=AXIS2_PLACEMENT_3D('',#35936,#28336,#28337);
#25654=AXIS2_PLACEMENT_3D('',#35940,#28339,#28340);
#25655=AXIS2_PLACEMENT_3D('',#35941,#28341,#28342);
#25656=AXIS2_PLACEMENT_3D('',#35942,#28343,#28344);
#25657=AXIS2_PLACEMENT_3D('',#35948,#28348,#28349);
#25658=AXIS2_PLACEMENT_3D('',#35949,#28350,#28351);
#25659=AXIS2_PLACEMENT_3D('',#35950,#28352,#28353);
#25660=AXIS2_PLACEMENT_3D('',#35951,#28354,#28355);
#25661=AXIS2_PLACEMENT_3D('',#35954,#28357,#28358);
#25662=AXIS2_PLACEMENT_3D('',#35955,#28359,#28360);
#25663=AXIS2_PLACEMENT_3D('',#35959,#28363,#28364);
#25664=AXIS2_PLACEMENT_3D('',#35960,#28365,#28366);
#25665=AXIS2_PLACEMENT_3D('',#35961,#28367,#28368);
#25666=AXIS2_PLACEMENT_3D('',#35964,#28370,#28371);
#25667=AXIS2_PLACEMENT_3D('',#35965,#28372,#28373);
#25668=AXIS2_PLACEMENT_3D('',#35969,#28376,#28377);
#25669=AXIS2_PLACEMENT_3D('',#35970,#28378,#28379);
#25670=AXIS2_PLACEMENT_3D('',#35971,#28380,#28381);
#25671=AXIS2_PLACEMENT_3D('',#35973,#28382,#28383);
#25672=AXIS2_PLACEMENT_3D('',#35974,#28384,#28385);
#25673=AXIS2_PLACEMENT_3D('',#35977,#28387,#28388);
#25674=AXIS2_PLACEMENT_3D('',#35978,#28389,#28390);
#25675=AXIS2_PLACEMENT_3D('',#35980,#28392,#28393);
#25676=AXIS2_PLACEMENT_3D('',#35983,#28395,#28396);
#25677=AXIS2_PLACEMENT_3D('',#35984,#28397,#28398);
#25678=AXIS2_PLACEMENT_3D('',#35986,#28400,#28401);
#25679=AXIS2_PLACEMENT_3D('',#35987,#28402,#28403);
#25680=AXIS2_PLACEMENT_3D('',#35989,#28405,#28406);
#25681=AXIS2_PLACEMENT_3D('',#35990,#28407,#28408);
#25682=AXIS2_PLACEMENT_3D('',#35993,#28410,#28411);
#25683=AXIS2_PLACEMENT_3D('',#35994,#28412,#28413);
#25684=AXIS2_PLACEMENT_3D('',#35995,#28414,#28415);
#25685=AXIS2_PLACEMENT_3D('',#35998,#28417,#28418);
#25686=AXIS2_PLACEMENT_3D('',#35999,#28419,#28420);
#25687=AXIS2_PLACEMENT_3D('',#36000,#28421,#28422);
#25688=AXIS2_PLACEMENT_3D('',#36002,#28423,#28424);
#25689=AXIS2_PLACEMENT_3D('',#36004,#28426,#28427);
#25690=AXIS2_PLACEMENT_3D('',#36006,#28428,#28429);
#25691=AXIS2_PLACEMENT_3D('',#36008,#28431,#28432);
#25692=AXIS2_PLACEMENT_3D('',#36010,#28433,#28434);
#25693=AXIS2_PLACEMENT_3D('',#36012,#28436,#28437);
#25694=AXIS2_PLACEMENT_3D('',#36014,#28438,#28439);
#25695=AXIS2_PLACEMENT_3D('',#36016,#28441,#28442);
#25696=AXIS2_PLACEMENT_3D('',#36017,#28443,#28444);
#25697=AXIS2_PLACEMENT_3D('',#36018,#28445,#28446);
#25698=AXIS2_PLACEMENT_3D('',#36019,#28447,#28448);
#25699=AXIS2_PLACEMENT_3D('',#36020,#28449,#28450);
#25700=AXIS2_PLACEMENT_3D('',#36022,#28452,#28453);
#25701=AXIS2_PLACEMENT_3D('',#36024,#28455,#28456);
#25702=AXIS2_PLACEMENT_3D('',#36026,#28458,#28459);
#25703=AXIS2_PLACEMENT_3D('',#36027,#28460,#28461);
#25704=AXIS2_PLACEMENT_3D('',#36028,#28462,#28463);
#25705=AXIS2_PLACEMENT_3D('',#36041,#28470,#28471);
#25706=AXIS2_PLACEMENT_3D('',#36520,#28711,#28712);
#25707=AXIS2_PLACEMENT_3D('',#36521,#28713,#28714);
#25708=AXIS2_PLACEMENT_3D('',#36529,#28719,#28720);
#25709=AXIS2_PLACEMENT_3D('',#36533,#28723,#28724);
#25710=AXIS2_PLACEMENT_3D('',#36543,#28730,#28731);
#25711=AXIS2_PLACEMENT_3D('',#36551,#28736,#28737);
#25712=AXIS2_PLACEMENT_3D('',#36555,#28740,#28741);
#25713=AXIS2_PLACEMENT_3D('',#36565,#28747,#28748);
#25714=AXIS2_PLACEMENT_3D('',#36573,#28753,#28754);
#25715=AXIS2_PLACEMENT_3D('',#36577,#28757,#28758);
#25716=AXIS2_PLACEMENT_3D('',#36587,#28764,#28765);
#25717=AXIS2_PLACEMENT_3D('',#36595,#28770,#28771);
#25718=AXIS2_PLACEMENT_3D('',#36599,#28774,#28775);
#25719=AXIS2_PLACEMENT_3D('',#36609,#28781,#28782);
#25720=AXIS2_PLACEMENT_3D('',#36617,#28787,#28788);
#25721=AXIS2_PLACEMENT_3D('',#36621,#28791,#28792);
#25722=AXIS2_PLACEMENT_3D('',#36631,#28798,#28799);
#25723=AXIS2_PLACEMENT_3D('',#36639,#28804,#28805);
#25724=AXIS2_PLACEMENT_3D('',#36643,#28808,#28809);
#25725=AXIS2_PLACEMENT_3D('',#36653,#28815,#28816);
#25726=AXIS2_PLACEMENT_3D('',#36661,#28821,#28822);
#25727=AXIS2_PLACEMENT_3D('',#36665,#28825,#28826);
#25728=AXIS2_PLACEMENT_3D('',#36675,#28832,#28833);
#25729=AXIS2_PLACEMENT_3D('',#36683,#28838,#28839);
#25730=AXIS2_PLACEMENT_3D('',#36687,#28842,#28843);
#25731=AXIS2_PLACEMENT_3D('',#36697,#28849,#28850);
#25732=AXIS2_PLACEMENT_3D('',#36705,#28855,#28856);
#25733=AXIS2_PLACEMENT_3D('',#36709,#28859,#28860);
#25734=AXIS2_PLACEMENT_3D('',#36719,#28866,#28867);
#25735=AXIS2_PLACEMENT_3D('',#36727,#28872,#28873);
#25736=AXIS2_PLACEMENT_3D('',#36731,#28876,#28877);
#25737=AXIS2_PLACEMENT_3D('',#36741,#28883,#28884);
#25738=AXIS2_PLACEMENT_3D('',#36749,#28889,#28890);
#25739=AXIS2_PLACEMENT_3D('',#36753,#28893,#28894);
#25740=AXIS2_PLACEMENT_3D('',#36763,#28900,#28901);
#25741=AXIS2_PLACEMENT_3D('',#36771,#28906,#28907);
#25742=AXIS2_PLACEMENT_3D('',#36775,#28910,#28911);
#25743=AXIS2_PLACEMENT_3D('',#36785,#28917,#28918);
#25744=AXIS2_PLACEMENT_3D('',#36791,#28922,#28923);
#25745=AXIS2_PLACEMENT_3D('',#36795,#28926,#28927);
#25746=AXIS2_PLACEMENT_3D('',#36805,#28933,#28934);
#25747=AXIS2_PLACEMENT_3D('',#36811,#28938,#28939);
#25748=AXIS2_PLACEMENT_3D('',#36815,#28942,#28943);
#25749=AXIS2_PLACEMENT_3D('',#36825,#28949,#28950);
#25750=AXIS2_PLACEMENT_3D('',#36831,#28954,#28955);
#25751=AXIS2_PLACEMENT_3D('',#36835,#28958,#28959);
#25752=AXIS2_PLACEMENT_3D('',#36845,#28965,#28966);
#25753=AXIS2_PLACEMENT_3D('',#36851,#28970,#28971);
#25754=AXIS2_PLACEMENT_3D('',#36855,#28974,#28975);
#25755=AXIS2_PLACEMENT_3D('',#36865,#28981,#28982);
#25756=AXIS2_PLACEMENT_3D('',#36871,#28986,#28987);
#25757=AXIS2_PLACEMENT_3D('',#36875,#28990,#28991);
#25758=AXIS2_PLACEMENT_3D('',#36885,#28997,#28998);
#25759=AXIS2_PLACEMENT_3D('',#36891,#29002,#29003);
#25760=AXIS2_PLACEMENT_3D('',#36895,#29006,#29007);
#25761=AXIS2_PLACEMENT_3D('',#36905,#29013,#29014);
#25762=AXIS2_PLACEMENT_3D('',#36911,#29018,#29019);
#25763=AXIS2_PLACEMENT_3D('',#36915,#29022,#29023);
#25764=AXIS2_PLACEMENT_3D('',#36925,#29029,#29030);
#25765=AXIS2_PLACEMENT_3D('',#36931,#29034,#29035);
#25766=AXIS2_PLACEMENT_3D('',#36935,#29038,#29039);
#25767=AXIS2_PLACEMENT_3D('',#36945,#29045,#29046);
#25768=AXIS2_PLACEMENT_3D('',#36951,#29050,#29051);
#25769=AXIS2_PLACEMENT_3D('',#36955,#29054,#29055);
#25770=AXIS2_PLACEMENT_3D('',#36965,#29061,#29062);
#25771=AXIS2_PLACEMENT_3D('',#36971,#29066,#29067);
#25772=AXIS2_PLACEMENT_3D('',#36975,#29070,#29071);
#25773=AXIS2_PLACEMENT_3D('',#36985,#29077,#29078);
#25774=AXIS2_PLACEMENT_3D('',#36991,#29082,#29083);
#25775=AXIS2_PLACEMENT_3D('',#36995,#29086,#29087);
#25776=AXIS2_PLACEMENT_3D('',#37005,#29093,#29094);
#25777=AXIS2_PLACEMENT_3D('',#37011,#29098,#29099);
#25778=AXIS2_PLACEMENT_3D('',#37015,#29102,#29103);
#25779=AXIS2_PLACEMENT_3D('',#37023,#29108,#29109);
#25780=AXIS2_PLACEMENT_3D('',#37467,#29337,#29338);
#25781=AXIS2_PLACEMENT_3D('',#37468,#29339,#29340);
#25782=AXIS2_PLACEMENT_3D('',#37473,#29344,#29345);
#25783=AXIS2_PLACEMENT_3D('',#37479,#29349,#29350);
#25784=AXIS2_PLACEMENT_3D('',#37484,#29354,#29355);
#25785=AXIS2_PLACEMENT_3D('',#37490,#29359,#29360);
#25786=AXIS2_PLACEMENT_3D('',#37495,#29364,#29365);
#25787=AXIS2_PLACEMENT_3D('',#37501,#29369,#29370);
#25788=AXIS2_PLACEMENT_3D('',#37506,#29374,#29375);
#25789=AXIS2_PLACEMENT_3D('',#37512,#29379,#29380);
#25790=AXIS2_PLACEMENT_3D('',#37517,#29384,#29385);
#25791=AXIS2_PLACEMENT_3D('',#37523,#29389,#29390);
#25792=AXIS2_PLACEMENT_3D('',#37528,#29394,#29395);
#25793=AXIS2_PLACEMENT_3D('',#37534,#29399,#29400);
#25794=AXIS2_PLACEMENT_3D('',#37539,#29404,#29405);
#25795=AXIS2_PLACEMENT_3D('',#37545,#29409,#29410);
#25796=AXIS2_PLACEMENT_3D('',#37550,#29414,#29415);
#25797=AXIS2_PLACEMENT_3D('',#37556,#29419,#29420);
#25798=AXIS2_PLACEMENT_3D('',#37561,#29424,#29425);
#25799=AXIS2_PLACEMENT_3D('',#37567,#29429,#29430);
#25800=AXIS2_PLACEMENT_3D('',#37572,#29434,#29435);
#25801=AXIS2_PLACEMENT_3D('',#37578,#29439,#29440);
#25802=AXIS2_PLACEMENT_3D('',#37583,#29444,#29445);
#25803=AXIS2_PLACEMENT_3D('',#37589,#29449,#29450);
#25804=AXIS2_PLACEMENT_3D('',#37594,#29454,#29455);
#25805=AXIS2_PLACEMENT_3D('',#37597,#29456,#29457);
#25806=AXIS2_PLACEMENT_3D('',#37603,#29461,#29462);
#25807=AXIS2_PLACEMENT_3D('',#37609,#29466,#29467);
#25808=AXIS2_PLACEMENT_3D('',#37615,#29471,#29472);
#25809=AXIS2_PLACEMENT_3D('',#37616,#29473,#29474);
#25810=AXIS2_PLACEMENT_3D('',#37618,#29476,#29477);
#25811=AXIS2_PLACEMENT_3D('',#37619,#29478,#29479);
#25812=AXIS2_PLACEMENT_3D('',#37622,#29482,#29483);
#25813=AXIS2_PLACEMENT_3D('',#37624,#29485,#29486);
#25814=AXIS2_PLACEMENT_3D('',#37625,#29487,#29488);
#25815=AXIS2_PLACEMENT_3D('',#37627,#29490,#29491);
#25816=AXIS2_PLACEMENT_3D('',#37629,#29493,#29494);
#25817=AXIS2_PLACEMENT_3D('',#37631,#29496,#29497);
#25818=AXIS2_PLACEMENT_3D('',#37633,#29499,#29500);
#25819=AXIS2_PLACEMENT_3D('',#37635,#29502,#29503);
#25820=AXIS2_PLACEMENT_3D('',#37637,#29505,#29506);
#25821=AXIS2_PLACEMENT_3D('',#37639,#29508,#29509);
#25822=AXIS2_PLACEMENT_3D('',#37641,#29511,#29512);
#25823=AXIS2_PLACEMENT_3D('',#37643,#29514,#29515);
#25824=AXIS2_PLACEMENT_3D('',#37645,#29517,#29518);
#25825=AXIS2_PLACEMENT_3D('',#37647,#29520,#29521);
#25826=AXIS2_PLACEMENT_3D('',#37649,#29523,#29524);
#25827=AXIS2_PLACEMENT_3D('',#37651,#29526,#29527);
#25828=AXIS2_PLACEMENT_3D('',#37653,#29529,#29530);
#25829=AXIS2_PLACEMENT_3D('',#37655,#29532,#29533);
#25830=AXIS2_PLACEMENT_3D('',#37656,#29534,#29535);
#25831=AXIS2_PLACEMENT_3D('',#37658,#29537,#29538);
#25832=AXIS2_PLACEMENT_3D('',#37660,#29540,#29541);
#25833=AXIS2_PLACEMENT_3D('',#37662,#29543,#29544);
#25834=AXIS2_PLACEMENT_3D('',#37663,#29545,#29546);
#25835=AXIS2_PLACEMENT_3D('',#37665,#29548,#29549);
#25836=AXIS2_PLACEMENT_3D('',#37667,#29551,#29552);
#25837=AXIS2_PLACEMENT_3D('',#37669,#29554,#29555);
#25838=AXIS2_PLACEMENT_3D('',#37671,#29557,#29558);
#25839=AXIS2_PLACEMENT_3D('',#37673,#29560,#29561);
#25840=AXIS2_PLACEMENT_3D('',#37675,#29563,#29564);
#25841=AXIS2_PLACEMENT_3D('',#37677,#29566,#29567);
#25842=AXIS2_PLACEMENT_3D('',#37679,#29569,#29570);
#25843=AXIS2_PLACEMENT_3D('',#37681,#29572,#29573);
#25844=AXIS2_PLACEMENT_3D('',#37683,#29575,#29576);
#25845=AXIS2_PLACEMENT_3D('',#37685,#29578,#29579);
#25846=AXIS2_PLACEMENT_3D('',#37687,#29581,#29582);
#25847=AXIS2_PLACEMENT_3D('',#37689,#29584,#29585);
#25848=AXIS2_PLACEMENT_3D('',#37691,#29587,#29588);
#25849=AXIS2_PLACEMENT_3D('',#37693,#29590,#29591);
#25850=AXIS2_PLACEMENT_3D('',#37694,#29592,#29593);
#25851=AXIS2_PLACEMENT_3D('',#37696,#29595,#29596);
#25852=AXIS2_PLACEMENT_3D('',#37698,#29598,#29599);
#25853=AXIS2_PLACEMENT_3D('',#37700,#29601,#29602);
#25854=AXIS2_PLACEMENT_3D('',#37701,#29603,#29604);
#25855=AXIS2_PLACEMENT_3D('',#37703,#29606,#29607);
#25856=AXIS2_PLACEMENT_3D('',#37705,#29609,#29610);
#25857=AXIS2_PLACEMENT_3D('',#37707,#29612,#29613);
#25858=AXIS2_PLACEMENT_3D('',#37709,#29615,#29616);
#25859=AXIS2_PLACEMENT_3D('',#37711,#29618,#29619);
#25860=AXIS2_PLACEMENT_3D('',#37713,#29621,#29622);
#25861=AXIS2_PLACEMENT_3D('',#37715,#29624,#29625);
#25862=AXIS2_PLACEMENT_3D('',#37717,#29627,#29628);
#25863=AXIS2_PLACEMENT_3D('',#37719,#29630,#29631);
#25864=AXIS2_PLACEMENT_3D('',#37721,#29633,#29634);
#25865=AXIS2_PLACEMENT_3D('',#37723,#29636,#29637);
#25866=AXIS2_PLACEMENT_3D('',#37725,#29639,#29640);
#25867=AXIS2_PLACEMENT_3D('',#37727,#29642,#29643);
#25868=AXIS2_PLACEMENT_3D('',#37729,#29645,#29646);
#25869=AXIS2_PLACEMENT_3D('',#37731,#29648,#29649);
#25870=AXIS2_PLACEMENT_3D('',#37732,#29650,#29651);
#25871=AXIS2_PLACEMENT_3D('',#37734,#29653,#29654);
#25872=AXIS2_PLACEMENT_3D('',#37736,#29656,#29657);
#25873=AXIS2_PLACEMENT_3D('',#37738,#29659,#29660);
#25874=AXIS2_PLACEMENT_3D('',#37739,#29661,#29662);
#25875=AXIS2_PLACEMENT_3D('',#37741,#29664,#29665);
#25876=AXIS2_PLACEMENT_3D('',#37743,#29667,#29668);
#25877=AXIS2_PLACEMENT_3D('',#37745,#29670,#29671);
#25878=AXIS2_PLACEMENT_3D('',#37747,#29673,#29674);
#25879=AXIS2_PLACEMENT_3D('',#37749,#29676,#29677);
#25880=AXIS2_PLACEMENT_3D('',#37751,#29679,#29680);
#25881=AXIS2_PLACEMENT_3D('',#37753,#29682,#29683);
#25882=AXIS2_PLACEMENT_3D('',#37755,#29685,#29686);
#25883=AXIS2_PLACEMENT_3D('',#37757,#29688,#29689);
#25884=AXIS2_PLACEMENT_3D('',#37759,#29691,#29692);
#25885=AXIS2_PLACEMENT_3D('',#37761,#29694,#29695);
#25886=AXIS2_PLACEMENT_3D('',#37763,#29697,#29698);
#25887=AXIS2_PLACEMENT_3D('',#37765,#29700,#29701);
#25888=AXIS2_PLACEMENT_3D('',#37767,#29703,#29704);
#25889=AXIS2_PLACEMENT_3D('',#37769,#29706,#29707);
#25890=AXIS2_PLACEMENT_3D('',#37770,#29708,#29709);
#25891=AXIS2_PLACEMENT_3D('',#37772,#29711,#29712);
#25892=AXIS2_PLACEMENT_3D('',#37774,#29714,#29715);
#25893=AXIS2_PLACEMENT_3D('',#37776,#29717,#29718);
#25894=AXIS2_PLACEMENT_3D('',#37777,#29719,#29720);
#25895=AXIS2_PLACEMENT_3D('',#37779,#29722,#29723);
#25896=AXIS2_PLACEMENT_3D('',#37781,#29725,#29726);
#25897=AXIS2_PLACEMENT_3D('',#37783,#29728,#29729);
#25898=AXIS2_PLACEMENT_3D('',#37785,#29731,#29732);
#25899=AXIS2_PLACEMENT_3D('',#37787,#29734,#29735);
#25900=AXIS2_PLACEMENT_3D('',#37789,#29737,#29738);
#25901=AXIS2_PLACEMENT_3D('',#37791,#29740,#29741);
#25902=AXIS2_PLACEMENT_3D('',#37793,#29743,#29744);
#25903=AXIS2_PLACEMENT_3D('',#37795,#29746,#29747);
#25904=AXIS2_PLACEMENT_3D('',#37797,#29749,#29750);
#25905=AXIS2_PLACEMENT_3D('',#37799,#29752,#29753);
#25906=AXIS2_PLACEMENT_3D('',#37801,#29755,#29756);
#25907=AXIS2_PLACEMENT_3D('',#37803,#29758,#29759);
#25908=AXIS2_PLACEMENT_3D('',#37805,#29761,#29762);
#25909=AXIS2_PLACEMENT_3D('',#37807,#29764,#29765);
#25910=AXIS2_PLACEMENT_3D('',#37808,#29766,#29767);
#25911=AXIS2_PLACEMENT_3D('',#37810,#29769,#29770);
#25912=AXIS2_PLACEMENT_3D('',#37812,#29772,#29773);
#25913=AXIS2_PLACEMENT_3D('',#37814,#29775,#29776);
#25914=AXIS2_PLACEMENT_3D('',#37815,#29777,#29778);
#25915=AXIS2_PLACEMENT_3D('',#37817,#29780,#29781);
#25916=AXIS2_PLACEMENT_3D('',#37819,#29783,#29784);
#25917=AXIS2_PLACEMENT_3D('',#37821,#29786,#29787);
#25918=AXIS2_PLACEMENT_3D('',#37823,#29789,#29790);
#25919=AXIS2_PLACEMENT_3D('',#37825,#29792,#29793);
#25920=AXIS2_PLACEMENT_3D('',#37827,#29795,#29796);
#25921=AXIS2_PLACEMENT_3D('',#37829,#29798,#29799);
#25922=AXIS2_PLACEMENT_3D('',#37831,#29801,#29802);
#25923=AXIS2_PLACEMENT_3D('',#37833,#29804,#29805);
#25924=AXIS2_PLACEMENT_3D('',#37835,#29807,#29808);
#25925=AXIS2_PLACEMENT_3D('',#37837,#29810,#29811);
#25926=AXIS2_PLACEMENT_3D('',#37839,#29813,#29814);
#25927=AXIS2_PLACEMENT_3D('',#37841,#29816,#29817);
#25928=AXIS2_PLACEMENT_3D('',#37843,#29819,#29820);
#25929=AXIS2_PLACEMENT_3D('',#37845,#29822,#29823);
#25930=AXIS2_PLACEMENT_3D('',#37846,#29824,#29825);
#25931=AXIS2_PLACEMENT_3D('',#37848,#29827,#29828);
#25932=AXIS2_PLACEMENT_3D('',#37850,#29830,#29831);
#25933=AXIS2_PLACEMENT_3D('',#37852,#29833,#29834);
#25934=AXIS2_PLACEMENT_3D('',#37853,#29835,#29836);
#25935=AXIS2_PLACEMENT_3D('',#37855,#29838,#29839);
#25936=AXIS2_PLACEMENT_3D('',#37857,#29841,#29842);
#25937=AXIS2_PLACEMENT_3D('',#37859,#29844,#29845);
#25938=AXIS2_PLACEMENT_3D('',#37861,#29847,#29848);
#25939=AXIS2_PLACEMENT_3D('',#37863,#29850,#29851);
#25940=AXIS2_PLACEMENT_3D('',#37865,#29853,#29854);
#25941=AXIS2_PLACEMENT_3D('',#37867,#29856,#29857);
#25942=AXIS2_PLACEMENT_3D('',#37869,#29859,#29860);
#25943=AXIS2_PLACEMENT_3D('',#37871,#29862,#29863);
#25944=AXIS2_PLACEMENT_3D('',#37873,#29865,#29866);
#25945=AXIS2_PLACEMENT_3D('',#37875,#29868,#29869);
#25946=AXIS2_PLACEMENT_3D('',#37877,#29871,#29872);
#25947=AXIS2_PLACEMENT_3D('',#37879,#29874,#29875);
#25948=AXIS2_PLACEMENT_3D('',#37881,#29877,#29878);
#25949=AXIS2_PLACEMENT_3D('',#37883,#29880,#29881);
#25950=AXIS2_PLACEMENT_3D('',#37884,#29882,#29883);
#25951=AXIS2_PLACEMENT_3D('',#37886,#29885,#29886);
#25952=AXIS2_PLACEMENT_3D('',#37888,#29888,#29889);
#25953=AXIS2_PLACEMENT_3D('',#37890,#29891,#29892);
#25954=AXIS2_PLACEMENT_3D('',#37891,#29893,#29894);
#25955=AXIS2_PLACEMENT_3D('',#37893,#29896,#29897);
#25956=AXIS2_PLACEMENT_3D('',#37895,#29899,#29900);
#25957=AXIS2_PLACEMENT_3D('',#37897,#29902,#29903);
#25958=AXIS2_PLACEMENT_3D('',#37899,#29905,#29906);
#25959=AXIS2_PLACEMENT_3D('',#37901,#29908,#29909);
#25960=AXIS2_PLACEMENT_3D('',#37903,#29911,#29912);
#25961=AXIS2_PLACEMENT_3D('',#37905,#29914,#29915);
#25962=AXIS2_PLACEMENT_3D('',#37907,#29917,#29918);
#25963=AXIS2_PLACEMENT_3D('',#37909,#29920,#29921);
#25964=AXIS2_PLACEMENT_3D('',#37911,#29923,#29924);
#25965=AXIS2_PLACEMENT_3D('',#37913,#29926,#29927);
#25966=AXIS2_PLACEMENT_3D('',#37915,#29929,#29930);
#25967=AXIS2_PLACEMENT_3D('',#37917,#29932,#29933);
#25968=AXIS2_PLACEMENT_3D('',#37919,#29935,#29936);
#25969=AXIS2_PLACEMENT_3D('',#37921,#29938,#29939);
#25970=AXIS2_PLACEMENT_3D('',#37922,#29940,#29941);
#25971=AXIS2_PLACEMENT_3D('',#37924,#29943,#29944);
#25972=AXIS2_PLACEMENT_3D('',#37926,#29946,#29947);
#25973=AXIS2_PLACEMENT_3D('',#37928,#29949,#29950);
#25974=AXIS2_PLACEMENT_3D('',#37929,#29951,#29952);
#25975=AXIS2_PLACEMENT_3D('',#37931,#29954,#29955);
#25976=AXIS2_PLACEMENT_3D('',#37933,#29957,#29958);
#25977=AXIS2_PLACEMENT_3D('',#37935,#29960,#29961);
#25978=AXIS2_PLACEMENT_3D('',#37937,#29963,#29964);
#25979=AXIS2_PLACEMENT_3D('',#37939,#29966,#29967);
#25980=AXIS2_PLACEMENT_3D('',#37941,#29969,#29970);
#25981=AXIS2_PLACEMENT_3D('',#37943,#29972,#29973);
#25982=AXIS2_PLACEMENT_3D('',#37945,#29975,#29976);
#25983=AXIS2_PLACEMENT_3D('',#37947,#29978,#29979);
#25984=AXIS2_PLACEMENT_3D('',#37949,#29981,#29982);
#25985=AXIS2_PLACEMENT_3D('',#37951,#29984,#29985);
#25986=AXIS2_PLACEMENT_3D('',#37953,#29987,#29988);
#25987=AXIS2_PLACEMENT_3D('',#37955,#29990,#29991);
#25988=AXIS2_PLACEMENT_3D('',#37957,#29993,#29994);
#25989=AXIS2_PLACEMENT_3D('',#37959,#29996,#29997);
#25990=AXIS2_PLACEMENT_3D('',#37960,#29998,#29999);
#25991=AXIS2_PLACEMENT_3D('',#37962,#30001,#30002);
#25992=AXIS2_PLACEMENT_3D('',#37964,#30004,#30005);
#25993=AXIS2_PLACEMENT_3D('',#37966,#30007,#30008);
#25994=AXIS2_PLACEMENT_3D('',#37967,#30009,#30010);
#25995=AXIS2_PLACEMENT_3D('',#37969,#30012,#30013);
#25996=AXIS2_PLACEMENT_3D('',#37971,#30015,#30016);
#25997=AXIS2_PLACEMENT_3D('',#37973,#30018,#30019);
#25998=AXIS2_PLACEMENT_3D('',#37975,#30021,#30022);
#25999=AXIS2_PLACEMENT_3D('',#37977,#30024,#30025);
#26000=AXIS2_PLACEMENT_3D('',#37979,#30027,#30028);
#26001=AXIS2_PLACEMENT_3D('',#37981,#30030,#30031);
#26002=AXIS2_PLACEMENT_3D('',#37983,#30033,#30034);
#26003=AXIS2_PLACEMENT_3D('',#37985,#30036,#30037);
#26004=AXIS2_PLACEMENT_3D('',#37987,#30039,#30040);
#26005=AXIS2_PLACEMENT_3D('',#37989,#30042,#30043);
#26006=AXIS2_PLACEMENT_3D('',#37991,#30045,#30046);
#26007=AXIS2_PLACEMENT_3D('',#37993,#30048,#30049);
#26008=AXIS2_PLACEMENT_3D('',#37995,#30051,#30052);
#26009=AXIS2_PLACEMENT_3D('',#37997,#30054,#30055);
#26010=AXIS2_PLACEMENT_3D('',#37998,#30056,#30057);
#26011=AXIS2_PLACEMENT_3D('',#38000,#30059,#30060);
#26012=AXIS2_PLACEMENT_3D('',#38002,#30062,#30063);
#26013=AXIS2_PLACEMENT_3D('',#38004,#30065,#30066);
#26014=AXIS2_PLACEMENT_3D('',#38005,#30067,#30068);
#26015=AXIS2_PLACEMENT_3D('',#38007,#30070,#30071);
#26016=AXIS2_PLACEMENT_3D('',#38009,#30073,#30074);
#26017=AXIS2_PLACEMENT_3D('',#38011,#30076,#30077);
#26018=AXIS2_PLACEMENT_3D('',#38013,#30079,#30080);
#26019=AXIS2_PLACEMENT_3D('',#38015,#30082,#30083);
#26020=AXIS2_PLACEMENT_3D('',#38017,#30085,#30086);
#26021=AXIS2_PLACEMENT_3D('',#38019,#30088,#30089);
#26022=AXIS2_PLACEMENT_3D('',#38021,#30091,#30092);
#26023=AXIS2_PLACEMENT_3D('',#38023,#30094,#30095);
#26024=AXIS2_PLACEMENT_3D('',#38025,#30097,#30098);
#26025=AXIS2_PLACEMENT_3D('',#38027,#30100,#30101);
#26026=AXIS2_PLACEMENT_3D('',#38029,#30103,#30104);
#26027=AXIS2_PLACEMENT_3D('',#38031,#30106,#30107);
#26028=AXIS2_PLACEMENT_3D('',#38033,#30109,#30110);
#26029=AXIS2_PLACEMENT_3D('',#38035,#30112,#30113);
#26030=AXIS2_PLACEMENT_3D('',#38036,#30114,#30115);
#26031=AXIS2_PLACEMENT_3D('',#38038,#30117,#30118);
#26032=AXIS2_PLACEMENT_3D('',#38040,#30120,#30121);
#26033=AXIS2_PLACEMENT_3D('',#38042,#30123,#30124);
#26034=AXIS2_PLACEMENT_3D('',#38043,#30125,#30126);
#26035=AXIS2_PLACEMENT_3D('',#38045,#30128,#30129);
#26036=AXIS2_PLACEMENT_3D('',#38047,#30131,#30132);
#26037=AXIS2_PLACEMENT_3D('',#38049,#30134,#30135);
#26038=AXIS2_PLACEMENT_3D('',#38051,#30137,#30138);
#26039=AXIS2_PLACEMENT_3D('',#38053,#30140,#30141);
#26040=AXIS2_PLACEMENT_3D('',#38055,#30143,#30144);
#26041=AXIS2_PLACEMENT_3D('',#38057,#30146,#30147);
#26042=AXIS2_PLACEMENT_3D('',#38059,#30149,#30150);
#26043=AXIS2_PLACEMENT_3D('',#38061,#30152,#30153);
#26044=AXIS2_PLACEMENT_3D('',#38063,#30155,#30156);
#26045=AXIS2_PLACEMENT_3D('',#38065,#30158,#30159);
#26046=AXIS2_PLACEMENT_3D('',#38067,#30161,#30162);
#26047=AXIS2_PLACEMENT_3D('',#38069,#30164,#30165);
#26048=AXIS2_PLACEMENT_3D('',#38071,#30167,#30168);
#26049=AXIS2_PLACEMENT_3D('',#38073,#30170,#30171);
#26050=AXIS2_PLACEMENT_3D('',#38074,#30172,#30173);
#26051=AXIS2_PLACEMENT_3D('',#38075,#30174,#30175);
#26052=AXIS2_PLACEMENT_3D('',#38078,#30177,#30178);
#26053=AXIS2_PLACEMENT_3D('',#38079,#30179,#30180);
#26054=AXIS2_PLACEMENT_3D('',#38081,#30181,#30182);
#26055=AXIS2_PLACEMENT_3D('',#38082,#30183,#30184);
#26056=AXIS2_PLACEMENT_3D('',#38084,#30185,#30186);
#26057=AXIS2_PLACEMENT_3D('',#38086,#30188,#30189);
#26058=AXIS2_PLACEMENT_3D('',#38088,#30190,#30191);
#26059=AXIS2_PLACEMENT_3D('',#38090,#30193,#30194);
#26060=AXIS2_PLACEMENT_3D('',#38091,#30195,#30196);
#26061=AXIS2_PLACEMENT_3D('',#38093,#30197,#30198);
#26062=AXIS2_PLACEMENT_3D('',#38095,#30200,#30201);
#26063=AXIS2_PLACEMENT_3D('',#38096,#30202,#30203);
#26064=AXIS2_PLACEMENT_3D('',#38097,#30204,#30205);
#26065=AXIS2_PLACEMENT_3D('',#38110,#30212,#30213);
#26066=AXIS2_PLACEMENT_3D('',#38589,#30453,#30454);
#26067=AXIS2_PLACEMENT_3D('',#38590,#30455,#30456);
#26068=AXIS2_PLACEMENT_3D('',#38598,#30461,#30462);
#26069=AXIS2_PLACEMENT_3D('',#38602,#30465,#30466);
#26070=AXIS2_PLACEMENT_3D('',#38612,#30472,#30473);
#26071=AXIS2_PLACEMENT_3D('',#38620,#30478,#30479);
#26072=AXIS2_PLACEMENT_3D('',#38624,#30482,#30483);
#26073=AXIS2_PLACEMENT_3D('',#38634,#30489,#30490);
#26074=AXIS2_PLACEMENT_3D('',#38642,#30495,#30496);
#26075=AXIS2_PLACEMENT_3D('',#38646,#30499,#30500);
#26076=AXIS2_PLACEMENT_3D('',#38656,#30506,#30507);
#26077=AXIS2_PLACEMENT_3D('',#38664,#30512,#30513);
#26078=AXIS2_PLACEMENT_3D('',#38668,#30516,#30517);
#26079=AXIS2_PLACEMENT_3D('',#38678,#30523,#30524);
#26080=AXIS2_PLACEMENT_3D('',#38686,#30529,#30530);
#26081=AXIS2_PLACEMENT_3D('',#38690,#30533,#30534);
#26082=AXIS2_PLACEMENT_3D('',#38700,#30540,#30541);
#26083=AXIS2_PLACEMENT_3D('',#38708,#30546,#30547);
#26084=AXIS2_PLACEMENT_3D('',#38712,#30550,#30551);
#26085=AXIS2_PLACEMENT_3D('',#38722,#30557,#30558);
#26086=AXIS2_PLACEMENT_3D('',#38730,#30563,#30564);
#26087=AXIS2_PLACEMENT_3D('',#38734,#30567,#30568);
#26088=AXIS2_PLACEMENT_3D('',#38744,#30574,#30575);
#26089=AXIS2_PLACEMENT_3D('',#38752,#30580,#30581);
#26090=AXIS2_PLACEMENT_3D('',#38756,#30584,#30585);
#26091=AXIS2_PLACEMENT_3D('',#38766,#30591,#30592);
#26092=AXIS2_PLACEMENT_3D('',#38774,#30597,#30598);
#26093=AXIS2_PLACEMENT_3D('',#38778,#30601,#30602);
#26094=AXIS2_PLACEMENT_3D('',#38788,#30608,#30609);
#26095=AXIS2_PLACEMENT_3D('',#38796,#30614,#30615);
#26096=AXIS2_PLACEMENT_3D('',#38800,#30618,#30619);
#26097=AXIS2_PLACEMENT_3D('',#38810,#30625,#30626);
#26098=AXIS2_PLACEMENT_3D('',#38818,#30631,#30632);
#26099=AXIS2_PLACEMENT_3D('',#38822,#30635,#30636);
#26100=AXIS2_PLACEMENT_3D('',#38832,#30642,#30643);
#26101=AXIS2_PLACEMENT_3D('',#38840,#30648,#30649);
#26102=AXIS2_PLACEMENT_3D('',#38844,#30652,#30653);
#26103=AXIS2_PLACEMENT_3D('',#38854,#30659,#30660);
#26104=AXIS2_PLACEMENT_3D('',#38860,#30664,#30665);
#26105=AXIS2_PLACEMENT_3D('',#38864,#30668,#30669);
#26106=AXIS2_PLACEMENT_3D('',#38874,#30675,#30676);
#26107=AXIS2_PLACEMENT_3D('',#38880,#30680,#30681);
#26108=AXIS2_PLACEMENT_3D('',#38884,#30684,#30685);
#26109=AXIS2_PLACEMENT_3D('',#38894,#30691,#30692);
#26110=AXIS2_PLACEMENT_3D('',#38900,#30696,#30697);
#26111=AXIS2_PLACEMENT_3D('',#38904,#30700,#30701);
#26112=AXIS2_PLACEMENT_3D('',#38914,#30707,#30708);
#26113=AXIS2_PLACEMENT_3D('',#38920,#30712,#30713);
#26114=AXIS2_PLACEMENT_3D('',#38924,#30716,#30717);
#26115=AXIS2_PLACEMENT_3D('',#38934,#30723,#30724);
#26116=AXIS2_PLACEMENT_3D('',#38940,#30728,#30729);
#26117=AXIS2_PLACEMENT_3D('',#38944,#30732,#30733);
#26118=AXIS2_PLACEMENT_3D('',#38954,#30739,#30740);
#26119=AXIS2_PLACEMENT_3D('',#38960,#30744,#30745);
#26120=AXIS2_PLACEMENT_3D('',#38964,#30748,#30749);
#26121=AXIS2_PLACEMENT_3D('',#38974,#30755,#30756);
#26122=AXIS2_PLACEMENT_3D('',#38980,#30760,#30761);
#26123=AXIS2_PLACEMENT_3D('',#38984,#30764,#30765);
#26124=AXIS2_PLACEMENT_3D('',#38994,#30771,#30772);
#26125=AXIS2_PLACEMENT_3D('',#39000,#30776,#30777);
#26126=AXIS2_PLACEMENT_3D('',#39004,#30780,#30781);
#26127=AXIS2_PLACEMENT_3D('',#39014,#30787,#30788);
#26128=AXIS2_PLACEMENT_3D('',#39020,#30792,#30793);
#26129=AXIS2_PLACEMENT_3D('',#39024,#30796,#30797);
#26130=AXIS2_PLACEMENT_3D('',#39034,#30803,#30804);
#26131=AXIS2_PLACEMENT_3D('',#39040,#30808,#30809);
#26132=AXIS2_PLACEMENT_3D('',#39044,#30812,#30813);
#26133=AXIS2_PLACEMENT_3D('',#39054,#30819,#30820);
#26134=AXIS2_PLACEMENT_3D('',#39060,#30824,#30825);
#26135=AXIS2_PLACEMENT_3D('',#39064,#30828,#30829);
#26136=AXIS2_PLACEMENT_3D('',#39074,#30835,#30836);
#26137=AXIS2_PLACEMENT_3D('',#39080,#30840,#30841);
#26138=AXIS2_PLACEMENT_3D('',#39084,#30844,#30845);
#26139=AXIS2_PLACEMENT_3D('',#39092,#30850,#30851);
#26140=AXIS2_PLACEMENT_3D('',#39536,#31079,#31080);
#26141=AXIS2_PLACEMENT_3D('',#39537,#31081,#31082);
#26142=AXIS2_PLACEMENT_3D('',#39542,#31086,#31087);
#26143=AXIS2_PLACEMENT_3D('',#39548,#31091,#31092);
#26144=AXIS2_PLACEMENT_3D('',#39553,#31096,#31097);
#26145=AXIS2_PLACEMENT_3D('',#39559,#31101,#31102);
#26146=AXIS2_PLACEMENT_3D('',#39564,#31106,#31107);
#26147=AXIS2_PLACEMENT_3D('',#39570,#31111,#31112);
#26148=AXIS2_PLACEMENT_3D('',#39575,#31116,#31117);
#26149=AXIS2_PLACEMENT_3D('',#39581,#31121,#31122);
#26150=AXIS2_PLACEMENT_3D('',#39586,#31126,#31127);
#26151=AXIS2_PLACEMENT_3D('',#39592,#31131,#31132);
#26152=AXIS2_PLACEMENT_3D('',#39597,#31136,#31137);
#26153=AXIS2_PLACEMENT_3D('',#39603,#31141,#31142);
#26154=AXIS2_PLACEMENT_3D('',#39608,#31146,#31147);
#26155=AXIS2_PLACEMENT_3D('',#39614,#31151,#31152);
#26156=AXIS2_PLACEMENT_3D('',#39619,#31156,#31157);
#26157=AXIS2_PLACEMENT_3D('',#39625,#31161,#31162);
#26158=AXIS2_PLACEMENT_3D('',#39630,#31166,#31167);
#26159=AXIS2_PLACEMENT_3D('',#39636,#31171,#31172);
#26160=AXIS2_PLACEMENT_3D('',#39641,#31176,#31177);
#26161=AXIS2_PLACEMENT_3D('',#39647,#31181,#31182);
#26162=AXIS2_PLACEMENT_3D('',#39652,#31186,#31187);
#26163=AXIS2_PLACEMENT_3D('',#39658,#31191,#31192);
#26164=AXIS2_PLACEMENT_3D('',#39663,#31196,#31197);
#26165=AXIS2_PLACEMENT_3D('',#39666,#31200,#31201);
#26166=AXIS2_PLACEMENT_3D('',#39668,#31203,#31204);
#26167=AXIS2_PLACEMENT_3D('',#39669,#31205,#31206);
#26168=AXIS2_PLACEMENT_3D('',#39671,#31208,#31209);
#26169=AXIS2_PLACEMENT_3D('',#39673,#31211,#31212);
#26170=AXIS2_PLACEMENT_3D('',#39675,#31214,#31215);
#26171=AXIS2_PLACEMENT_3D('',#39677,#31217,#31218);
#26172=AXIS2_PLACEMENT_3D('',#39679,#31220,#31221);
#26173=AXIS2_PLACEMENT_3D('',#39681,#31223,#31224);
#26174=AXIS2_PLACEMENT_3D('',#39683,#31226,#31227);
#26175=AXIS2_PLACEMENT_3D('',#39685,#31229,#31230);
#26176=AXIS2_PLACEMENT_3D('',#39687,#31232,#31233);
#26177=AXIS2_PLACEMENT_3D('',#39689,#31235,#31236);
#26178=AXIS2_PLACEMENT_3D('',#39691,#31238,#31239);
#26179=AXIS2_PLACEMENT_3D('',#39693,#31241,#31242);
#26180=AXIS2_PLACEMENT_3D('',#39695,#31244,#31245);
#26181=AXIS2_PLACEMENT_3D('',#39697,#31247,#31248);
#26182=AXIS2_PLACEMENT_3D('',#39699,#31250,#31251);
#26183=AXIS2_PLACEMENT_3D('',#39700,#31252,#31253);
#26184=AXIS2_PLACEMENT_3D('',#39702,#31255,#31256);
#26185=AXIS2_PLACEMENT_3D('',#39704,#31258,#31259);
#26186=AXIS2_PLACEMENT_3D('',#39706,#31261,#31262);
#26187=AXIS2_PLACEMENT_3D('',#39707,#31263,#31264);
#26188=AXIS2_PLACEMENT_3D('',#39709,#31266,#31267);
#26189=AXIS2_PLACEMENT_3D('',#39711,#31269,#31270);
#26190=AXIS2_PLACEMENT_3D('',#39713,#31272,#31273);
#26191=AXIS2_PLACEMENT_3D('',#39715,#31275,#31276);
#26192=AXIS2_PLACEMENT_3D('',#39717,#31278,#31279);
#26193=AXIS2_PLACEMENT_3D('',#39719,#31281,#31282);
#26194=AXIS2_PLACEMENT_3D('',#39721,#31284,#31285);
#26195=AXIS2_PLACEMENT_3D('',#39723,#31287,#31288);
#26196=AXIS2_PLACEMENT_3D('',#39725,#31290,#31291);
#26197=AXIS2_PLACEMENT_3D('',#39727,#31293,#31294);
#26198=AXIS2_PLACEMENT_3D('',#39729,#31296,#31297);
#26199=AXIS2_PLACEMENT_3D('',#39731,#31299,#31300);
#26200=AXIS2_PLACEMENT_3D('',#39733,#31302,#31303);
#26201=AXIS2_PLACEMENT_3D('',#39735,#31305,#31306);
#26202=AXIS2_PLACEMENT_3D('',#39737,#31308,#31309);
#26203=AXIS2_PLACEMENT_3D('',#39738,#31310,#31311);
#26204=AXIS2_PLACEMENT_3D('',#39740,#31313,#31314);
#26205=AXIS2_PLACEMENT_3D('',#39742,#31316,#31317);
#26206=AXIS2_PLACEMENT_3D('',#39744,#31319,#31320);
#26207=AXIS2_PLACEMENT_3D('',#39745,#31321,#31322);
#26208=AXIS2_PLACEMENT_3D('',#39747,#31324,#31325);
#26209=AXIS2_PLACEMENT_3D('',#39749,#31327,#31328);
#26210=AXIS2_PLACEMENT_3D('',#39751,#31330,#31331);
#26211=AXIS2_PLACEMENT_3D('',#39753,#31333,#31334);
#26212=AXIS2_PLACEMENT_3D('',#39755,#31336,#31337);
#26213=AXIS2_PLACEMENT_3D('',#39757,#31339,#31340);
#26214=AXIS2_PLACEMENT_3D('',#39759,#31342,#31343);
#26215=AXIS2_PLACEMENT_3D('',#39761,#31345,#31346);
#26216=AXIS2_PLACEMENT_3D('',#39763,#31348,#31349);
#26217=AXIS2_PLACEMENT_3D('',#39765,#31351,#31352);
#26218=AXIS2_PLACEMENT_3D('',#39767,#31354,#31355);
#26219=AXIS2_PLACEMENT_3D('',#39769,#31357,#31358);
#26220=AXIS2_PLACEMENT_3D('',#39771,#31360,#31361);
#26221=AXIS2_PLACEMENT_3D('',#39773,#31363,#31364);
#26222=AXIS2_PLACEMENT_3D('',#39775,#31366,#31367);
#26223=AXIS2_PLACEMENT_3D('',#39776,#31368,#31369);
#26224=AXIS2_PLACEMENT_3D('',#39778,#31371,#31372);
#26225=AXIS2_PLACEMENT_3D('',#39780,#31374,#31375);
#26226=AXIS2_PLACEMENT_3D('',#39782,#31377,#31378);
#26227=AXIS2_PLACEMENT_3D('',#39783,#31379,#31380);
#26228=AXIS2_PLACEMENT_3D('',#39785,#31382,#31383);
#26229=AXIS2_PLACEMENT_3D('',#39787,#31385,#31386);
#26230=AXIS2_PLACEMENT_3D('',#39789,#31388,#31389);
#26231=AXIS2_PLACEMENT_3D('',#39791,#31391,#31392);
#26232=AXIS2_PLACEMENT_3D('',#39793,#31394,#31395);
#26233=AXIS2_PLACEMENT_3D('',#39795,#31397,#31398);
#26234=AXIS2_PLACEMENT_3D('',#39797,#31400,#31401);
#26235=AXIS2_PLACEMENT_3D('',#39799,#31403,#31404);
#26236=AXIS2_PLACEMENT_3D('',#39801,#31406,#31407);
#26237=AXIS2_PLACEMENT_3D('',#39803,#31409,#31410);
#26238=AXIS2_PLACEMENT_3D('',#39805,#31412,#31413);
#26239=AXIS2_PLACEMENT_3D('',#39807,#31415,#31416);
#26240=AXIS2_PLACEMENT_3D('',#39809,#31418,#31419);
#26241=AXIS2_PLACEMENT_3D('',#39811,#31421,#31422);
#26242=AXIS2_PLACEMENT_3D('',#39813,#31424,#31425);
#26243=AXIS2_PLACEMENT_3D('',#39814,#31426,#31427);
#26244=AXIS2_PLACEMENT_3D('',#39816,#31429,#31430);
#26245=AXIS2_PLACEMENT_3D('',#39818,#31432,#31433);
#26246=AXIS2_PLACEMENT_3D('',#39820,#31435,#31436);
#26247=AXIS2_PLACEMENT_3D('',#39821,#31437,#31438);
#26248=AXIS2_PLACEMENT_3D('',#39823,#31440,#31441);
#26249=AXIS2_PLACEMENT_3D('',#39825,#31443,#31444);
#26250=AXIS2_PLACEMENT_3D('',#39827,#31446,#31447);
#26251=AXIS2_PLACEMENT_3D('',#39829,#31449,#31450);
#26252=AXIS2_PLACEMENT_3D('',#39831,#31452,#31453);
#26253=AXIS2_PLACEMENT_3D('',#39833,#31455,#31456);
#26254=AXIS2_PLACEMENT_3D('',#39835,#31458,#31459);
#26255=AXIS2_PLACEMENT_3D('',#39837,#31461,#31462);
#26256=AXIS2_PLACEMENT_3D('',#39839,#31464,#31465);
#26257=AXIS2_PLACEMENT_3D('',#39841,#31467,#31468);
#26258=AXIS2_PLACEMENT_3D('',#39843,#31470,#31471);
#26259=AXIS2_PLACEMENT_3D('',#39845,#31473,#31474);
#26260=AXIS2_PLACEMENT_3D('',#39847,#31476,#31477);
#26261=AXIS2_PLACEMENT_3D('',#39849,#31479,#31480);
#26262=AXIS2_PLACEMENT_3D('',#39851,#31482,#31483);
#26263=AXIS2_PLACEMENT_3D('',#39852,#31484,#31485);
#26264=AXIS2_PLACEMENT_3D('',#39854,#31487,#31488);
#26265=AXIS2_PLACEMENT_3D('',#39856,#31490,#31491);
#26266=AXIS2_PLACEMENT_3D('',#39858,#31493,#31494);
#26267=AXIS2_PLACEMENT_3D('',#39859,#31495,#31496);
#26268=AXIS2_PLACEMENT_3D('',#39861,#31498,#31499);
#26269=AXIS2_PLACEMENT_3D('',#39863,#31501,#31502);
#26270=AXIS2_PLACEMENT_3D('',#39865,#31504,#31505);
#26271=AXIS2_PLACEMENT_3D('',#39867,#31507,#31508);
#26272=AXIS2_PLACEMENT_3D('',#39869,#31510,#31511);
#26273=AXIS2_PLACEMENT_3D('',#39871,#31513,#31514);
#26274=AXIS2_PLACEMENT_3D('',#39873,#31516,#31517);
#26275=AXIS2_PLACEMENT_3D('',#39875,#31519,#31520);
#26276=AXIS2_PLACEMENT_3D('',#39877,#31522,#31523);
#26277=AXIS2_PLACEMENT_3D('',#39879,#31525,#31526);
#26278=AXIS2_PLACEMENT_3D('',#39881,#31528,#31529);
#26279=AXIS2_PLACEMENT_3D('',#39883,#31531,#31532);
#26280=AXIS2_PLACEMENT_3D('',#39885,#31534,#31535);
#26281=AXIS2_PLACEMENT_3D('',#39887,#31537,#31538);
#26282=AXIS2_PLACEMENT_3D('',#39889,#31540,#31541);
#26283=AXIS2_PLACEMENT_3D('',#39890,#31542,#31543);
#26284=AXIS2_PLACEMENT_3D('',#39892,#31545,#31546);
#26285=AXIS2_PLACEMENT_3D('',#39894,#31548,#31549);
#26286=AXIS2_PLACEMENT_3D('',#39896,#31551,#31552);
#26287=AXIS2_PLACEMENT_3D('',#39897,#31553,#31554);
#26288=AXIS2_PLACEMENT_3D('',#39899,#31556,#31557);
#26289=AXIS2_PLACEMENT_3D('',#39901,#31559,#31560);
#26290=AXIS2_PLACEMENT_3D('',#39903,#31562,#31563);
#26291=AXIS2_PLACEMENT_3D('',#39905,#31565,#31566);
#26292=AXIS2_PLACEMENT_3D('',#39907,#31568,#31569);
#26293=AXIS2_PLACEMENT_3D('',#39909,#31571,#31572);
#26294=AXIS2_PLACEMENT_3D('',#39911,#31574,#31575);
#26295=AXIS2_PLACEMENT_3D('',#39913,#31577,#31578);
#26296=AXIS2_PLACEMENT_3D('',#39915,#31580,#31581);
#26297=AXIS2_PLACEMENT_3D('',#39917,#31583,#31584);
#26298=AXIS2_PLACEMENT_3D('',#39919,#31586,#31587);
#26299=AXIS2_PLACEMENT_3D('',#39921,#31589,#31590);
#26300=AXIS2_PLACEMENT_3D('',#39923,#31592,#31593);
#26301=AXIS2_PLACEMENT_3D('',#39925,#31595,#31596);
#26302=AXIS2_PLACEMENT_3D('',#39927,#31598,#31599);
#26303=AXIS2_PLACEMENT_3D('',#39928,#31600,#31601);
#26304=AXIS2_PLACEMENT_3D('',#39930,#31603,#31604);
#26305=AXIS2_PLACEMENT_3D('',#39932,#31606,#31607);
#26306=AXIS2_PLACEMENT_3D('',#39934,#31609,#31610);
#26307=AXIS2_PLACEMENT_3D('',#39935,#31611,#31612);
#26308=AXIS2_PLACEMENT_3D('',#39937,#31614,#31615);
#26309=AXIS2_PLACEMENT_3D('',#39939,#31617,#31618);
#26310=AXIS2_PLACEMENT_3D('',#39941,#31620,#31621);
#26311=AXIS2_PLACEMENT_3D('',#39943,#31623,#31624);
#26312=AXIS2_PLACEMENT_3D('',#39945,#31626,#31627);
#26313=AXIS2_PLACEMENT_3D('',#39947,#31629,#31630);
#26314=AXIS2_PLACEMENT_3D('',#39949,#31632,#31633);
#26315=AXIS2_PLACEMENT_3D('',#39951,#31635,#31636);
#26316=AXIS2_PLACEMENT_3D('',#39953,#31638,#31639);
#26317=AXIS2_PLACEMENT_3D('',#39955,#31641,#31642);
#26318=AXIS2_PLACEMENT_3D('',#39957,#31644,#31645);
#26319=AXIS2_PLACEMENT_3D('',#39959,#31647,#31648);
#26320=AXIS2_PLACEMENT_3D('',#39961,#31650,#31651);
#26321=AXIS2_PLACEMENT_3D('',#39963,#31653,#31654);
#26322=AXIS2_PLACEMENT_3D('',#39965,#31656,#31657);
#26323=AXIS2_PLACEMENT_3D('',#39966,#31658,#31659);
#26324=AXIS2_PLACEMENT_3D('',#39968,#31661,#31662);
#26325=AXIS2_PLACEMENT_3D('',#39970,#31664,#31665);
#26326=AXIS2_PLACEMENT_3D('',#39972,#31667,#31668);
#26327=AXIS2_PLACEMENT_3D('',#39973,#31669,#31670);
#26328=AXIS2_PLACEMENT_3D('',#39975,#31672,#31673);
#26329=AXIS2_PLACEMENT_3D('',#39977,#31675,#31676);
#26330=AXIS2_PLACEMENT_3D('',#39979,#31678,#31679);
#26331=AXIS2_PLACEMENT_3D('',#39981,#31681,#31682);
#26332=AXIS2_PLACEMENT_3D('',#39983,#31684,#31685);
#26333=AXIS2_PLACEMENT_3D('',#39985,#31687,#31688);
#26334=AXIS2_PLACEMENT_3D('',#39987,#31690,#31691);
#26335=AXIS2_PLACEMENT_3D('',#39989,#31693,#31694);
#26336=AXIS2_PLACEMENT_3D('',#39991,#31696,#31697);
#26337=AXIS2_PLACEMENT_3D('',#39993,#31699,#31700);
#26338=AXIS2_PLACEMENT_3D('',#39995,#31702,#31703);
#26339=AXIS2_PLACEMENT_3D('',#39997,#31705,#31706);
#26340=AXIS2_PLACEMENT_3D('',#39999,#31708,#31709);
#26341=AXIS2_PLACEMENT_3D('',#40001,#31711,#31712);
#26342=AXIS2_PLACEMENT_3D('',#40003,#31714,#31715);
#26343=AXIS2_PLACEMENT_3D('',#40004,#31716,#31717);
#26344=AXIS2_PLACEMENT_3D('',#40006,#31719,#31720);
#26345=AXIS2_PLACEMENT_3D('',#40008,#31722,#31723);
#26346=AXIS2_PLACEMENT_3D('',#40010,#31725,#31726);
#26347=AXIS2_PLACEMENT_3D('',#40011,#31727,#31728);
#26348=AXIS2_PLACEMENT_3D('',#40013,#31730,#31731);
#26349=AXIS2_PLACEMENT_3D('',#40015,#31733,#31734);
#26350=AXIS2_PLACEMENT_3D('',#40017,#31736,#31737);
#26351=AXIS2_PLACEMENT_3D('',#40019,#31739,#31740);
#26352=AXIS2_PLACEMENT_3D('',#40021,#31742,#31743);
#26353=AXIS2_PLACEMENT_3D('',#40023,#31745,#31746);
#26354=AXIS2_PLACEMENT_3D('',#40025,#31748,#31749);
#26355=AXIS2_PLACEMENT_3D('',#40027,#31751,#31752);
#26356=AXIS2_PLACEMENT_3D('',#40029,#31754,#31755);
#26357=AXIS2_PLACEMENT_3D('',#40031,#31757,#31758);
#26358=AXIS2_PLACEMENT_3D('',#40033,#31760,#31761);
#26359=AXIS2_PLACEMENT_3D('',#40035,#31763,#31764);
#26360=AXIS2_PLACEMENT_3D('',#40037,#31766,#31767);
#26361=AXIS2_PLACEMENT_3D('',#40039,#31769,#31770);
#26362=AXIS2_PLACEMENT_3D('',#40041,#31772,#31773);
#26363=AXIS2_PLACEMENT_3D('',#40042,#31774,#31775);
#26364=AXIS2_PLACEMENT_3D('',#40044,#31777,#31778);
#26365=AXIS2_PLACEMENT_3D('',#40046,#31780,#31781);
#26366=AXIS2_PLACEMENT_3D('',#40048,#31783,#31784);
#26367=AXIS2_PLACEMENT_3D('',#40049,#31785,#31786);
#26368=AXIS2_PLACEMENT_3D('',#40051,#31788,#31789);
#26369=AXIS2_PLACEMENT_3D('',#40053,#31791,#31792);
#26370=AXIS2_PLACEMENT_3D('',#40055,#31794,#31795);
#26371=AXIS2_PLACEMENT_3D('',#40057,#31797,#31798);
#26372=AXIS2_PLACEMENT_3D('',#40059,#31800,#31801);
#26373=AXIS2_PLACEMENT_3D('',#40061,#31803,#31804);
#26374=AXIS2_PLACEMENT_3D('',#40063,#31806,#31807);
#26375=AXIS2_PLACEMENT_3D('',#40065,#31809,#31810);
#26376=AXIS2_PLACEMENT_3D('',#40067,#31812,#31813);
#26377=AXIS2_PLACEMENT_3D('',#40069,#31815,#31816);
#26378=AXIS2_PLACEMENT_3D('',#40071,#31818,#31819);
#26379=AXIS2_PLACEMENT_3D('',#40073,#31821,#31822);
#26380=AXIS2_PLACEMENT_3D('',#40075,#31824,#31825);
#26381=AXIS2_PLACEMENT_3D('',#40077,#31827,#31828);
#26382=AXIS2_PLACEMENT_3D('',#40079,#31830,#31831);
#26383=AXIS2_PLACEMENT_3D('',#40080,#31832,#31833);
#26384=AXIS2_PLACEMENT_3D('',#40082,#31835,#31836);
#26385=AXIS2_PLACEMENT_3D('',#40084,#31838,#31839);
#26386=AXIS2_PLACEMENT_3D('',#40086,#31841,#31842);
#26387=AXIS2_PLACEMENT_3D('',#40087,#31843,#31844);
#26388=AXIS2_PLACEMENT_3D('',#40089,#31846,#31847);
#26389=AXIS2_PLACEMENT_3D('',#40091,#31849,#31850);
#26390=AXIS2_PLACEMENT_3D('',#40093,#31852,#31853);
#26391=AXIS2_PLACEMENT_3D('',#40095,#31855,#31856);
#26392=AXIS2_PLACEMENT_3D('',#40097,#31858,#31859);
#26393=AXIS2_PLACEMENT_3D('',#40099,#31861,#31862);
#26394=AXIS2_PLACEMENT_3D('',#40101,#31864,#31865);
#26395=AXIS2_PLACEMENT_3D('',#40103,#31867,#31868);
#26396=AXIS2_PLACEMENT_3D('',#40105,#31870,#31871);
#26397=AXIS2_PLACEMENT_3D('',#40107,#31873,#31874);
#26398=AXIS2_PLACEMENT_3D('',#40109,#31876,#31877);
#26399=AXIS2_PLACEMENT_3D('',#40111,#31879,#31880);
#26400=AXIS2_PLACEMENT_3D('',#40113,#31882,#31883);
#26401=AXIS2_PLACEMENT_3D('',#40115,#31885,#31886);
#26402=AXIS2_PLACEMENT_3D('',#40117,#31888,#31889);
#26403=AXIS2_PLACEMENT_3D('',#40118,#31890,#31891);
#26404=AXIS2_PLACEMENT_3D('',#40119,#31892,#31893);
#26405=AXIS2_PLACEMENT_3D('',#40122,#31895,#31896);
#26406=AXIS2_PLACEMENT_3D('',#40123,#31897,#31898);
#26407=AXIS2_PLACEMENT_3D('',#40124,#31899,#31900);
#26408=AXIS2_PLACEMENT_3D('',#40126,#31901,#31902);
#26409=AXIS2_PLACEMENT_3D('',#40128,#31904,#31905);
#26410=AXIS2_PLACEMENT_3D('',#40129,#31906,#31907);
#26411=AXIS2_PLACEMENT_3D('',#40130,#31908,#31909);
#26412=AXIS2_PLACEMENT_3D('',#40139,#31914,#31915);
#26413=AXIS2_PLACEMENT_3D('',#40145,#31919,#31920);
#26414=AXIS2_PLACEMENT_3D('',#40151,#31924,#31925);
#26415=AXIS2_PLACEMENT_3D('',#40154,#31928,#31929);
#26416=AXIS2_PLACEMENT_3D('',#40155,#31930,#31931);
#26417=AXIS2_PLACEMENT_3D('',#40164,#31936,#31937);
#26418=AXIS2_PLACEMENT_3D('',#40170,#31941,#31942);
#26419=AXIS2_PLACEMENT_3D('',#40176,#31946,#31947);
#26420=AXIS2_PLACEMENT_3D('',#40179,#31950,#31951);
#26421=AXIS2_PLACEMENT_3D('',#40180,#31952,#31953);
#26422=AXIS2_PLACEMENT_3D('',#40182,#31954,#31955);
#26423=AXIS2_PLACEMENT_3D('',#40185,#31957,#31958);
#26424=AXIS2_PLACEMENT_3D('',#40186,#31959,#31960);
#26425=AXIS2_PLACEMENT_3D('',#40188,#31961,#31962);
#26426=AXIS2_PLACEMENT_3D('',#40191,#31964,#31965);
#26427=AXIS2_PLACEMENT_3D('',#40192,#31966,#31967);
#26428=AXIS2_PLACEMENT_3D('',#40195,#31968,#31969);
#26429=AXIS2_PLACEMENT_3D('',#40199,#31971,#31972);
#26430=AXIS2_PLACEMENT_3D('',#40201,#31974,#31975);
#26431=AXIS2_PLACEMENT_3D('',#40202,#31976,#31977);
#26432=AXIS2_PLACEMENT_3D('',#40203,#31978,#31979);
#26433=AXIS2_PLACEMENT_3D('',#40204,#31980,#31981);
#26434=AXIS2_PLACEMENT_3D('',#40205,#31982,#31983);
#26435=AXIS2_PLACEMENT_3D('',#40206,#31984,#31985);
#26436=AXIS2_PLACEMENT_3D('',#40207,#31986,#31987);
#26437=AXIS2_PLACEMENT_3D('',#40210,#31988,#31989);
#26438=AXIS2_PLACEMENT_3D('',#40211,#31990,#31991);
#26439=AXIS2_PLACEMENT_3D('',#40214,#31993,#31994);
#26440=AXIS2_PLACEMENT_3D('',#40215,#31995,#31996);
#26441=AXIS2_PLACEMENT_3D('',#40217,#31997,#31998);
#26442=AXIS2_PLACEMENT_3D('',#40218,#31999,#32000);
#26443=AXIS2_PLACEMENT_3D('',#40220,#32001,#32002);
#26444=AXIS2_PLACEMENT_3D('',#40222,#32004,#32005);
#26445=AXIS2_PLACEMENT_3D('',#40224,#32006,#32007);
#26446=AXIS2_PLACEMENT_3D('',#40226,#32009,#32010);
#26447=AXIS2_PLACEMENT_3D('',#40228,#32011,#32012);
#26448=AXIS2_PLACEMENT_3D('',#40229,#32013,#32014);
#26449=AXIS2_PLACEMENT_3D('',#40231,#32015,#32016);
#26450=AXIS2_PLACEMENT_3D('',#40233,#32018,#32019);
#26451=AXIS2_PLACEMENT_3D('',#40235,#32020,#32021);
#26452=AXIS2_PLACEMENT_3D('',#40236,#32022,#32023);
#26453=AXIS2_PLACEMENT_3D('',#40239,#32025,#32026);
#26454=AXIS2_PLACEMENT_3D('',#40240,#32027,#32028);
#26455=AXIS2_PLACEMENT_3D('',#40242,#32029,#32030);
#26456=AXIS2_PLACEMENT_3D('',#40243,#32031,#32032);
#26457=AXIS2_PLACEMENT_3D('',#40245,#32034,#32035);
#26458=AXIS2_PLACEMENT_3D('',#40246,#32036,#32037);
#26459=AXIS2_PLACEMENT_3D('',#40251,#32039,#32040);
#26460=AXIS2_PLACEMENT_3D('',#40258,#32042,#32043);
#26461=AXIS2_PLACEMENT_3D('',#40260,#32044,#32045);
#26462=AXIS2_PLACEMENT_3D('',#40262,#32046,#32047);
#26463=AXIS2_PLACEMENT_3D('',#40267,#32048,#32049);
#26464=AXIS2_PLACEMENT_3D('',#40271,#32051,#32052);
#26465=AXIS2_PLACEMENT_3D('',#40273,#32054,#32055);
#26466=AXIS2_PLACEMENT_3D('',#40279,#32059,#32060);
#26467=AXIS2_PLACEMENT_3D('',#40282,#32062,#32063);
#26468=AXIS2_PLACEMENT_3D('',#40283,#32064,#32065);
#26469=AXIS2_PLACEMENT_3D('',#40287,#32068,#32069);
#26470=AXIS2_PLACEMENT_3D('',#40289,#32070,#32071);
#26471=AXIS2_PLACEMENT_3D('',#40296,#32073,#32074);
#26472=AXIS2_PLACEMENT_3D('',#40298,#32075,#32076);
#26473=AXIS2_PLACEMENT_3D('',#40303,#32077,#32078);
#26474=AXIS2_PLACEMENT_3D('',#40306,#32080,#32081);
#26475=AXIS2_PLACEMENT_3D('',#40307,#32082,#32083);
#26476=AXIS2_PLACEMENT_3D('',#40308,#32084,#32085);
#26477=AXIS2_PLACEMENT_3D('',#40310,#32086,#32087);
#26478=AXIS2_PLACEMENT_3D('',#40312,#32088,#32089);
#26479=AXIS2_PLACEMENT_3D('',#40313,#32090,#32091);
#26480=AXIS2_PLACEMENT_3D('',#40314,#32092,#32093);
#26481=AXIS2_PLACEMENT_3D('',#40315,#32094,#32095);
#26482=AXIS2_PLACEMENT_3D('',#40318,#32097,#32098);
#26483=AXIS2_PLACEMENT_3D('',#40319,#32099,#32100);
#26484=AXIS2_PLACEMENT_3D('',#40322,#32102,#32103);
#26485=AXIS2_PLACEMENT_3D('',#40323,#32104,#32105);
#26486=AXIS2_PLACEMENT_3D('',#40325,#32106,#32107);
#26487=AXIS2_PLACEMENT_3D('',#40327,#32109,#32110);
#26488=AXIS2_PLACEMENT_3D('',#40329,#32111,#32112);
#26489=AXIS2_PLACEMENT_3D('',#40330,#32113,#32114);
#26490=AXIS2_PLACEMENT_3D('',#40333,#32116,#32117);
#26491=AXIS2_PLACEMENT_3D('',#40334,#32118,#32119);
#26492=AXIS2_PLACEMENT_3D('',#40337,#32121,#32122);
#26493=AXIS2_PLACEMENT_3D('',#40338,#32123,#32124);
#26494=AXIS2_PLACEMENT_3D('',#40340,#32126,#32127);
#26495=AXIS2_PLACEMENT_3D('',#40341,#32128,#32129);
#26496=AXIS2_PLACEMENT_3D('',#40354,#32136,#32137);
#26497=AXIS2_PLACEMENT_3D('',#40360,#32141,#32142);
#26498=AXIS2_PLACEMENT_3D('',#40368,#32147,#32148);
#26499=AXIS2_PLACEMENT_3D('',#40376,#32153,#32154);
#26500=AXIS2_PLACEMENT_3D('',#40386,#32160,#32161);
#26501=AXIS2_PLACEMENT_3D('',#40392,#32165,#32166);
#26502=AXIS2_PLACEMENT_3D('',#40400,#32171,#32172);
#26503=AXIS2_PLACEMENT_3D('',#40405,#32176,#32177);
#26504=AXIS2_PLACEMENT_3D('',#40409,#32180,#32181);
#26505=AXIS2_PLACEMENT_3D('',#40417,#32186,#32187);
#26506=AXIS2_PLACEMENT_3D('',#40422,#32191,#32192);
#26507=AXIS2_PLACEMENT_3D('',#40426,#32195,#32196);
#26508=AXIS2_PLACEMENT_3D('',#40432,#32200,#32201);
#26509=AXIS2_PLACEMENT_3D('',#40434,#32203,#32204);
#26510=AXIS2_PLACEMENT_3D('',#40436,#32206,#32207);
#26511=AXIS2_PLACEMENT_3D('',#40437,#32208,#32209);
#26512=AXIS2_PLACEMENT_3D('',#40438,#32210,#32211);
#26513=AXIS2_PLACEMENT_3D('',#40439,#32212,#32213);
#26514=AXIS2_PLACEMENT_3D('',#40440,#32214,#32215);
#26515=AXIS2_PLACEMENT_3D('',#40443,#32216,#32217);
#26516=AXIS2_PLACEMENT_3D('',#40444,#32218,#32219);
#26517=AXIS2_PLACEMENT_3D('',#40446,#32220,#32221);
#26518=AXIS2_PLACEMENT_3D('',#40448,#32222,#32223);
#26519=AXIS2_PLACEMENT_3D('',#40449,#32224,#32225);
#26520=AXIS2_PLACEMENT_3D('',#40450,#32226,#32227);
#26521=AXIS2_PLACEMENT_3D('',#40454,#32229,#32230);
#26522=AXIS2_PLACEMENT_3D('',#40455,#32231,#32232);
#26523=AXIS2_PLACEMENT_3D('',#40456,#32233,#32234);
#26524=AXIS2_PLACEMENT_3D('',#40458,#32235,#32236);
#26525=AXIS2_PLACEMENT_3D('',#40460,#32237,#32238);
#26526=AXIS2_PLACEMENT_3D('',#40461,#32239,#32240);
#26527=AXIS2_PLACEMENT_3D('',#40462,#32241,#32242);
#26528=AXIS2_PLACEMENT_3D('',#40464,#32244,#32245);
#26529=AXIS2_PLACEMENT_3D('',#40465,#32246,#32247);
#26530=AXIS2_PLACEMENT_3D('',#40472,#32251,#32252);
#26531=AXIS2_PLACEMENT_3D('',#40479,#32256,#32257);
#26532=AXIS2_PLACEMENT_3D('',#40486,#32261,#32262);
#26533=AXIS2_PLACEMENT_3D('',#40493,#32266,#32267);
#26534=AXIS2_PLACEMENT_3D('',#40496,#32270,#32271);
#26535=AXIS2_PLACEMENT_3D('',#40503,#32275,#32276);
#26536=AXIS2_PLACEMENT_3D('',#40510,#32280,#32281);
#26537=AXIS2_PLACEMENT_3D('',#40513,#32284,#32285);
#26538=AXIS2_PLACEMENT_3D('',#40516,#32288,#32289);
#26539=AXIS2_PLACEMENT_3D('',#40524,#32292,#32293);
#26540=AXIS2_PLACEMENT_3D('',#40527,#32296,#32297);
#26541=AXIS2_PLACEMENT_3D('',#40535,#32300,#32301);
#26542=AXIS2_PLACEMENT_3D('',#40543,#32304,#32305);
#26543=AXIS2_PLACEMENT_3D('',#40546,#32308,#32309);
#26544=AXIS2_PLACEMENT_3D('',#40554,#32312,#32313);
#26545=AXIS2_PLACEMENT_3D('',#40562,#32316,#32317);
#26546=AXIS2_PLACEMENT_3D('',#40565,#32320,#32321);
#26547=AXIS2_PLACEMENT_3D('',#40573,#32324,#32325);
#26548=AXIS2_PLACEMENT_3D('',#40577,#32326,#32327);
#26549=AXIS2_PLACEMENT_3D('',#40585,#32328,#32329);
#26550=AXIS2_PLACEMENT_3D('',#40589,#32330,#32331);
#26551=AXIS2_PLACEMENT_3D('',#40591,#32332,#32333);
#26552=AXIS2_PLACEMENT_3D('',#40592,#32334,#32335);
#26553=AXIS2_PLACEMENT_3D('',#40601,#32340,#32341);
#26554=AXIS2_PLACEMENT_3D('',#40607,#32345,#32346);
#26555=AXIS2_PLACEMENT_3D('',#40616,#32351,#32352);
#26556=AXIS2_PLACEMENT_3D('',#40622,#32356,#32357);
#26557=AXIS2_PLACEMENT_3D('',#40625,#32360,#32361);
#26558=AXIS2_PLACEMENT_3D('',#40628,#32364,#32365);
#26559=AXIS2_PLACEMENT_3D('',#40634,#32369,#32370);
#26560=AXIS2_PLACEMENT_3D('',#40638,#32373,#32374);
#26561=AXIS2_PLACEMENT_3D('',#40642,#32377,#32378);
#26562=AXIS2_PLACEMENT_3D('',#40644,#32379,#32380);
#26563=AXIS2_PLACEMENT_3D('',#40645,#32381,#32382);
#26564=AXIS2_PLACEMENT_3D('',#40649,#32385,#32386);
#26565=AXIS2_PLACEMENT_3D('',#40653,#32389,#32390);
#26566=AXIS2_PLACEMENT_3D('',#40655,#32392,#32393);
#26567=AXIS2_PLACEMENT_3D('',#40656,#32394,#32395);
#26568=AXIS2_PLACEMENT_3D('',#40667,#32397,#32398);
#26569=AXIS2_PLACEMENT_3D('',#40668,#32399,#32400);
#26570=AXIS2_PLACEMENT_3D('',#40669,#32401,#32402);
#26571=AXIS2_PLACEMENT_3D('',#40670,#32403,#32404);
#26572=AXIS2_PLACEMENT_3D('',#40672,#32405,#32406);
#26573=AXIS2_PLACEMENT_3D('',#40673,#32407,#32408);
#26574=AXIS2_PLACEMENT_3D('',#40675,#32409,#32410);
#26575=AXIS2_PLACEMENT_3D('',#40677,#32412,#32413);
#26576=AXIS2_PLACEMENT_3D('',#40679,#32414,#32415);
#26577=AXIS2_PLACEMENT_3D('',#40681,#32417,#32418);
#26578=AXIS2_PLACEMENT_3D('',#40683,#32419,#32420);
#26579=AXIS2_PLACEMENT_3D('',#40684,#32421,#32422);
#26580=AXIS2_PLACEMENT_3D('',#40686,#32424,#32425);
#26581=AXIS2_PLACEMENT_3D('',#40687,#32426,#32427);
#26582=AXIS2_PLACEMENT_3D('',#40689,#32428,#32429);
#26583=AXIS2_PLACEMENT_3D('',#40692,#32431,#32432);
#26584=AXIS2_PLACEMENT_3D('',#40693,#32433,#32434);
#26585=AXIS2_PLACEMENT_3D('',#40695,#32435,#32436);
#26586=AXIS2_PLACEMENT_3D('',#40696,#32437,#32438);
#26587=AXIS2_PLACEMENT_3D('',#40698,#32439,#32440);
#26588=AXIS2_PLACEMENT_3D('',#40699,#32441,#32442);
#26589=AXIS2_PLACEMENT_3D('',#40701,#32443,#32444);
#26590=AXIS2_PLACEMENT_3D('',#40703,#32446,#32447);
#26591=AXIS2_PLACEMENT_3D('',#40705,#32448,#32449);
#26592=AXIS2_PLACEMENT_3D('',#40708,#32451,#32452);
#26593=AXIS2_PLACEMENT_3D('',#40709,#32453,#32454);
#26594=AXIS2_PLACEMENT_3D('',#40711,#32455,#32456);
#26595=AXIS2_PLACEMENT_3D('',#40712,#32457,#32458);
#26596=AXIS2_PLACEMENT_3D('',#40714,#32459,#32460);
#26597=AXIS2_PLACEMENT_3D('',#40716,#32462,#32463);
#26598=AXIS2_PLACEMENT_3D('',#40718,#32464,#32465);
#26599=AXIS2_PLACEMENT_3D('',#40719,#32466,#32467);
#26600=AXIS2_PLACEMENT_3D('',#40722,#32469,#32470);
#26601=AXIS2_PLACEMENT_3D('',#40723,#32471,#32472);
#26602=AXIS2_PLACEMENT_3D('',#40724,#32473,#32474);
#26603=AXIS2_PLACEMENT_3D('',#40727,#32476,#32477);
#26604=AXIS2_PLACEMENT_3D('',#40728,#32478,#32479);
#26605=AXIS2_PLACEMENT_3D('',#40729,#32480,#32481);
#26606=AXIS2_PLACEMENT_3D('',#40730,#32482,#32483);
#26607=AXIS2_PLACEMENT_3D('',#40752,#32485,#32486);
#26608=AXIS2_PLACEMENT_3D('',#40763,#32487,#32488);
#26609=AXIS2_PLACEMENT_3D('',#40847,#32490,#32491);
#26610=AXIS2_PLACEMENT_3D('',#40937,#32493,#32494);
#26611=AXIS2_PLACEMENT_3D('',#41027,#32496,#32497);
#26612=AXIS2_PLACEMENT_3D('',#41111,#32499,#32500);
#26613=AXIS2_PLACEMENT_3D('',#41201,#32502,#32503);
#26614=AXIS2_PLACEMENT_3D('',#41291,#32505,#32506);
#26615=AXIS2_PLACEMENT_3D('',#41375,#32508,#32509);
#26616=AXIS2_PLACEMENT_3D('',#41465,#32511,#32512);
#26617=AXIS2_PLACEMENT_3D('',#41543,#32514,#32515);
#26618=AXIS2_PLACEMENT_3D('',#41591,#32517,#32518);
#26619=AXIS2_PLACEMENT_3D('',#41645,#32520,#32521);
#26620=AXIS2_PLACEMENT_3D('',#41729,#32523,#32524);
#26621=AXIS2_PLACEMENT_3D('',#41813,#32526,#32527);
#26622=AXIS2_PLACEMENT_3D('',#41903,#32529,#32530);
#26623=AXIS2_PLACEMENT_3D('',#41993,#32532,#32533);
#26624=AXIS2_PLACEMENT_3D('',#42077,#32535,#32536);
#26625=AXIS2_PLACEMENT_3D('',#42167,#32538,#32539);
#26626=AXIS2_PLACEMENT_3D('',#42257,#32541,#32542);
#26627=AXIS2_PLACEMENT_3D('',#42341,#32544,#32545);
#26628=AXIS2_PLACEMENT_3D('',#42346,#32547,#32548);
#26629=AXIS2_PLACEMENT_3D('',#42427,#32549,#32550);
#26630=AXIS2_PLACEMENT_3D('',#42444,#32552,#32553);
#26631=AXIS2_PLACEMENT_3D('',#42453,#32554,#32555);
#26632=AXIS2_PLACEMENT_3D('',#42490,#32557,#32558);
#26633=AXIS2_PLACEMENT_3D('',#42527,#32560,#32561);
#26634=AXIS2_PLACEMENT_3D('',#42565,#32563,#32564);
#26635=AXIS2_PLACEMENT_3D('',#42602,#32566,#32567);
#26636=AXIS2_PLACEMENT_3D('',#42639,#32569,#32570);
#26637=AXIS2_PLACEMENT_3D('',#42677,#32572,#32573);
#26638=AXIS2_PLACEMENT_3D('',#42714,#32575,#32576);
#26639=AXIS2_PLACEMENT_3D('',#42751,#32578,#32579);
#26640=AXIS2_PLACEMENT_3D('',#42782,#32581,#32582);
#26641=AXIS2_PLACEMENT_3D('',#42806,#32584,#32585);
#26642=AXIS2_PLACEMENT_3D('',#42834,#32587,#32588);
#26643=AXIS2_PLACEMENT_3D('',#42871,#32590,#32591);
#26644=AXIS2_PLACEMENT_3D('',#42908,#32593,#32594);
#26645=AXIS2_PLACEMENT_3D('',#42945,#32596,#32597);
#26646=AXIS2_PLACEMENT_3D('',#42983,#32599,#32600);
#26647=AXIS2_PLACEMENT_3D('',#43020,#32602,#32603);
#26648=AXIS2_PLACEMENT_3D('',#43057,#32605,#32606);
#26649=AXIS2_PLACEMENT_3D('',#43095,#32608,#32609);
#26650=AXIS2_PLACEMENT_3D('',#43132,#32611,#32612);
#26651=AXIS2_PLACEMENT_3D('',#43237,#32613,#32614);
#26652=AXIS2_PLACEMENT_3D('',#44451,#32615,#32616);
#26653=AXIS2_PLACEMENT_3D('',#44453,#32617,#32618);
#26654=AXIS2_PLACEMENT_3D('',#44454,#32619,#32620);
#26655=AXIS2_PLACEMENT_3D('',#44559,#32621,#32622);
#26656=AXIS2_PLACEMENT_3D('',#44560,#32623,#32624);
#26657=AXIS2_PLACEMENT_3D('',#45569,#32625,#32626);
#26658=AXIS2_PLACEMENT_3D('',#45578,#32631,#32632);
#26659=AXIS2_PLACEMENT_3D('',#45580,#32633,#32634);
#26660=AXIS2_PLACEMENT_3D('',#45582,#32636,#32637);
#26661=AXIS2_PLACEMENT_3D('',#45586,#32640,#32641);
#26662=AXIS2_PLACEMENT_3D('',#45587,#32642,#32643);
#26663=AXIS2_PLACEMENT_3D('',#45588,#32644,#32645);
#26664=AXIS2_PLACEMENT_3D('',#45597,#32650,#32651);
#26665=AXIS2_PLACEMENT_3D('',#45599,#32652,#32653);
#26666=AXIS2_PLACEMENT_3D('',#45601,#32655,#32656);
#26667=AXIS2_PLACEMENT_3D('',#45605,#32659,#32660);
#26668=AXIS2_PLACEMENT_3D('',#45606,#32661,#32662);
#26669=AXIS2_PLACEMENT_3D('',#45607,#32663,#32664);
#26670=AXIS2_PLACEMENT_3D('',#45616,#32669,#32670);
#26671=AXIS2_PLACEMENT_3D('',#45618,#32671,#32672);
#26672=AXIS2_PLACEMENT_3D('',#45620,#32674,#32675);
#26673=AXIS2_PLACEMENT_3D('',#45624,#32678,#32679);
#26674=AXIS2_PLACEMENT_3D('',#45625,#32680,#32681);
#26675=AXIS2_PLACEMENT_3D('',#45626,#32682,#32683);
#26676=AXIS2_PLACEMENT_3D('',#45635,#32688,#32689);
#26677=AXIS2_PLACEMENT_3D('',#45637,#32690,#32691);
#26678=AXIS2_PLACEMENT_3D('',#45639,#32693,#32694);
#26679=AXIS2_PLACEMENT_3D('',#45643,#32697,#32698);
#26680=AXIS2_PLACEMENT_3D('',#45644,#32699,#32700);
#26681=AXIS2_PLACEMENT_3D('',#45645,#32701,#32702);
#26682=AXIS2_PLACEMENT_3D('',#45654,#32707,#32708);
#26683=AXIS2_PLACEMENT_3D('',#45656,#32709,#32710);
#26684=AXIS2_PLACEMENT_3D('',#45658,#32712,#32713);
#26685=AXIS2_PLACEMENT_3D('',#45662,#32716,#32717);
#26686=AXIS2_PLACEMENT_3D('',#45663,#32718,#32719);
#26687=AXIS2_PLACEMENT_3D('',#45664,#32720,#32721);
#26688=AXIS2_PLACEMENT_3D('',#45673,#32726,#32727);
#26689=AXIS2_PLACEMENT_3D('',#45675,#32728,#32729);
#26690=AXIS2_PLACEMENT_3D('',#45677,#32731,#32732);
#26691=AXIS2_PLACEMENT_3D('',#45681,#32735,#32736);
#26692=AXIS2_PLACEMENT_3D('',#45682,#32737,#32738);
#26693=AXIS2_PLACEMENT_3D('',#45683,#32739,#32740);
#26694=AXIS2_PLACEMENT_3D('',#45692,#32745,#32746);
#26695=AXIS2_PLACEMENT_3D('',#45694,#32747,#32748);
#26696=AXIS2_PLACEMENT_3D('',#45696,#32750,#32751);
#26697=AXIS2_PLACEMENT_3D('',#45700,#32754,#32755);
#26698=AXIS2_PLACEMENT_3D('',#45701,#32756,#32757);
#26699=AXIS2_PLACEMENT_3D('',#45702,#32758,#32759);
#26700=AXIS2_PLACEMENT_3D('',#45711,#32764,#32765);
#26701=AXIS2_PLACEMENT_3D('',#45713,#32766,#32767);
#26702=AXIS2_PLACEMENT_3D('',#45715,#32769,#32770);
#26703=AXIS2_PLACEMENT_3D('',#45719,#32773,#32774);
#26704=AXIS2_PLACEMENT_3D('',#45720,#32775,#32776);
#26705=AXIS2_PLACEMENT_3D('',#45721,#32777,#32778);
#26706=AXIS2_PLACEMENT_3D('',#45730,#32783,#32784);
#26707=AXIS2_PLACEMENT_3D('',#45732,#32785,#32786);
#26708=AXIS2_PLACEMENT_3D('',#45734,#32788,#32789);
#26709=AXIS2_PLACEMENT_3D('',#45738,#32792,#32793);
#26710=AXIS2_PLACEMENT_3D('',#45739,#32794,#32795);
#26711=AXIS2_PLACEMENT_3D('',#45740,#32796,#32797);
#26712=AXIS2_PLACEMENT_3D('',#45749,#32802,#32803);
#26713=AXIS2_PLACEMENT_3D('',#45751,#32804,#32805);
#26714=AXIS2_PLACEMENT_3D('',#45753,#32807,#32808);
#26715=AXIS2_PLACEMENT_3D('',#45757,#32811,#32812);
#26716=AXIS2_PLACEMENT_3D('',#45758,#32813,#32814);
#26717=AXIS2_PLACEMENT_3D('',#45759,#32815,#32816);
#26718=AXIS2_PLACEMENT_3D('',#45768,#32821,#32822);
#26719=AXIS2_PLACEMENT_3D('',#45770,#32823,#32824);
#26720=AXIS2_PLACEMENT_3D('',#45772,#32826,#32827);
#26721=AXIS2_PLACEMENT_3D('',#45776,#32830,#32831);
#26722=AXIS2_PLACEMENT_3D('',#45777,#32832,#32833);
#26723=AXIS2_PLACEMENT_3D('',#45778,#32834,#32835);
#26724=AXIS2_PLACEMENT_3D('',#45787,#32840,#32841);
#26725=AXIS2_PLACEMENT_3D('',#45789,#32842,#32843);
#26726=AXIS2_PLACEMENT_3D('',#45791,#32845,#32846);
#26727=AXIS2_PLACEMENT_3D('',#45795,#32849,#32850);
#26728=AXIS2_PLACEMENT_3D('',#45796,#32851,#32852);
#26729=AXIS2_PLACEMENT_3D('',#45797,#32853,#32854);
#26730=AXIS2_PLACEMENT_3D('',#45806,#32859,#32860);
#26731=AXIS2_PLACEMENT_3D('',#45808,#32861,#32862);
#26732=AXIS2_PLACEMENT_3D('',#45810,#32864,#32865);
#26733=AXIS2_PLACEMENT_3D('',#45814,#32868,#32869);
#26734=AXIS2_PLACEMENT_3D('',#45815,#32870,#32871);
#26735=AXIS2_PLACEMENT_3D('',#45816,#32872,#32873);
#26736=AXIS2_PLACEMENT_3D('',#45825,#32878,#32879);
#26737=AXIS2_PLACEMENT_3D('',#45827,#32880,#32881);
#26738=AXIS2_PLACEMENT_3D('',#45829,#32883,#32884);
#26739=AXIS2_PLACEMENT_3D('',#45833,#32887,#32888);
#26740=AXIS2_PLACEMENT_3D('',#45834,#32889,#32890);
#26741=AXIS2_PLACEMENT_3D('',#45835,#32891,#32892);
#26742=AXIS2_PLACEMENT_3D('',#45844,#32897,#32898);
#26743=AXIS2_PLACEMENT_3D('',#45846,#32899,#32900);
#26744=AXIS2_PLACEMENT_3D('',#45848,#32902,#32903);
#26745=AXIS2_PLACEMENT_3D('',#45852,#32906,#32907);
#26746=AXIS2_PLACEMENT_3D('',#45853,#32908,#32909);
#26747=AXIS2_PLACEMENT_3D('',#45854,#32910,#32911);
#26748=AXIS2_PLACEMENT_3D('',#45863,#32916,#32917);
#26749=AXIS2_PLACEMENT_3D('',#45865,#32918,#32919);
#26750=AXIS2_PLACEMENT_3D('',#45867,#32921,#32922);
#26751=AXIS2_PLACEMENT_3D('',#45871,#32925,#32926);
#26752=AXIS2_PLACEMENT_3D('',#45872,#32927,#32928);
#26753=AXIS2_PLACEMENT_3D('',#45873,#32929,#32930);
#26754=AXIS2_PLACEMENT_3D('',#45882,#32935,#32936);
#26755=AXIS2_PLACEMENT_3D('',#45884,#32937,#32938);
#26756=AXIS2_PLACEMENT_3D('',#45886,#32940,#32941);
#26757=AXIS2_PLACEMENT_3D('',#45890,#32944,#32945);
#26758=AXIS2_PLACEMENT_3D('',#45891,#32946,#32947);
#26759=AXIS2_PLACEMENT_3D('',#45892,#32948,#32949);
#26760=AXIS2_PLACEMENT_3D('',#45901,#32954,#32955);
#26761=AXIS2_PLACEMENT_3D('',#45903,#32956,#32957);
#26762=AXIS2_PLACEMENT_3D('',#45906,#32959,#32960);
#26763=AXIS2_PLACEMENT_3D('',#45907,#32961,#32962);
#26764=AXIS2_PLACEMENT_3D('',#45911,#32965,#32966);
#26765=AXIS2_PLACEMENT_3D('',#45913,#32967,#32968);
#26766=AXIS2_PLACEMENT_3D('',#45914,#32969,#32970);
#26767=AXIS2_PLACEMENT_3D('',#45915,#32971,#32972);
#26768=AXIS2_PLACEMENT_3D('',#45924,#32977,#32978);
#26769=AXIS2_PLACEMENT_3D('',#45926,#32979,#32980);
#26770=AXIS2_PLACEMENT_3D('',#45928,#32982,#32983);
#26771=AXIS2_PLACEMENT_3D('',#45932,#32986,#32987);
#26772=AXIS2_PLACEMENT_3D('',#45933,#32988,#32989);
#26773=AXIS2_PLACEMENT_3D('',#45934,#32990,#32991);
#26774=AXIS2_PLACEMENT_3D('',#45943,#32996,#32997);
#26775=AXIS2_PLACEMENT_3D('',#45945,#32998,#32999);
#26776=AXIS2_PLACEMENT_3D('',#45947,#33001,#33002);
#26777=AXIS2_PLACEMENT_3D('',#45951,#33005,#33006);
#26778=AXIS2_PLACEMENT_3D('',#45952,#33007,#33008);
#26779=AXIS2_PLACEMENT_3D('',#45953,#33009,#33010);
#26780=AXIS2_PLACEMENT_3D('',#45962,#33015,#33016);
#26781=AXIS2_PLACEMENT_3D('',#45964,#33017,#33018);
#26782=AXIS2_PLACEMENT_3D('',#45966,#33020,#33021);
#26783=AXIS2_PLACEMENT_3D('',#45970,#33024,#33025);
#26784=AXIS2_PLACEMENT_3D('',#45971,#33026,#33027);
#26785=AXIS2_PLACEMENT_3D('',#45972,#33028,#33029);
#26786=AXIS2_PLACEMENT_3D('',#45981,#33034,#33035);
#26787=AXIS2_PLACEMENT_3D('',#45983,#33036,#33037);
#26788=AXIS2_PLACEMENT_3D('',#45985,#33039,#33040);
#26789=AXIS2_PLACEMENT_3D('',#45989,#33043,#33044);
#26790=AXIS2_PLACEMENT_3D('',#45990,#33045,#33046);
#26791=AXIS2_PLACEMENT_3D('',#45991,#33047,#33048);
#26792=AXIS2_PLACEMENT_3D('',#46000,#33053,#33054);
#26793=AXIS2_PLACEMENT_3D('',#46002,#33055,#33056);
#26794=AXIS2_PLACEMENT_3D('',#46004,#33058,#33059);
#26795=AXIS2_PLACEMENT_3D('',#46008,#33062,#33063);
#26796=AXIS2_PLACEMENT_3D('',#46009,#33064,#33065);
#26797=AXIS2_PLACEMENT_3D('',#46010,#33066,#33067);
#26798=AXIS2_PLACEMENT_3D('',#46019,#33072,#33073);
#26799=AXIS2_PLACEMENT_3D('',#46021,#33074,#33075);
#26800=AXIS2_PLACEMENT_3D('',#46023,#33077,#33078);
#26801=AXIS2_PLACEMENT_3D('',#46027,#33081,#33082);
#26802=AXIS2_PLACEMENT_3D('',#46028,#33083,#33084);
#26803=AXIS2_PLACEMENT_3D('',#46029,#33085,#33086);
#26804=AXIS2_PLACEMENT_3D('',#46038,#33091,#33092);
#26805=AXIS2_PLACEMENT_3D('',#46040,#33093,#33094);
#26806=AXIS2_PLACEMENT_3D('',#46042,#33096,#33097);
#26807=AXIS2_PLACEMENT_3D('',#46046,#33100,#33101);
#26808=AXIS2_PLACEMENT_3D('',#46047,#33102,#33103);
#26809=AXIS2_PLACEMENT_3D('',#46048,#33104,#33105);
#26810=AXIS2_PLACEMENT_3D('',#46057,#33110,#33111);
#26811=AXIS2_PLACEMENT_3D('',#46059,#33112,#33113);
#26812=AXIS2_PLACEMENT_3D('',#46061,#33115,#33116);
#26813=AXIS2_PLACEMENT_3D('',#46065,#33119,#33120);
#26814=AXIS2_PLACEMENT_3D('',#46066,#33121,#33122);
#26815=AXIS2_PLACEMENT_3D('',#46067,#33123,#33124);
#26816=AXIS2_PLACEMENT_3D('',#46076,#33129,#33130);
#26817=AXIS2_PLACEMENT_3D('',#46078,#33131,#33132);
#26818=AXIS2_PLACEMENT_3D('',#46080,#33134,#33135);
#26819=AXIS2_PLACEMENT_3D('',#46084,#33138,#33139);
#26820=AXIS2_PLACEMENT_3D('',#46085,#33140,#33141);
#26821=AXIS2_PLACEMENT_3D('',#46086,#33142,#33143);
#26822=AXIS2_PLACEMENT_3D('',#46095,#33148,#33149);
#26823=AXIS2_PLACEMENT_3D('',#46097,#33150,#33151);
#26824=AXIS2_PLACEMENT_3D('',#46099,#33153,#33154);
#26825=AXIS2_PLACEMENT_3D('',#46103,#33157,#33158);
#26826=AXIS2_PLACEMENT_3D('',#46104,#33159,#33160);
#26827=AXIS2_PLACEMENT_3D('',#46105,#33161,#33162);
#26828=AXIS2_PLACEMENT_3D('',#46114,#33167,#33168);
#26829=AXIS2_PLACEMENT_3D('',#46116,#33169,#33170);
#26830=AXIS2_PLACEMENT_3D('',#46118,#33172,#33173);
#26831=AXIS2_PLACEMENT_3D('',#46122,#33176,#33177);
#26832=AXIS2_PLACEMENT_3D('',#46123,#33178,#33179);
#26833=AXIS2_PLACEMENT_3D('',#46124,#33180,#33181);
#26834=AXIS2_PLACEMENT_3D('',#46133,#33186,#33187);
#26835=AXIS2_PLACEMENT_3D('',#46135,#33188,#33189);
#26836=AXIS2_PLACEMENT_3D('',#46137,#33191,#33192);
#26837=AXIS2_PLACEMENT_3D('',#46141,#33195,#33196);
#26838=AXIS2_PLACEMENT_3D('',#46142,#33197,#33198);
#26839=AXIS2_PLACEMENT_3D('',#46143,#33199,#33200);
#26840=AXIS2_PLACEMENT_3D('',#46152,#33205,#33206);
#26841=AXIS2_PLACEMENT_3D('',#46154,#33207,#33208);
#26842=AXIS2_PLACEMENT_3D('',#46156,#33210,#33211);
#26843=AXIS2_PLACEMENT_3D('',#46160,#33214,#33215);
#26844=AXIS2_PLACEMENT_3D('',#46161,#33216,#33217);
#26845=AXIS2_PLACEMENT_3D('',#46162,#33218,#33219);
#26846=AXIS2_PLACEMENT_3D('',#46171,#33224,#33225);
#26847=AXIS2_PLACEMENT_3D('',#46173,#33226,#33227);
#26848=AXIS2_PLACEMENT_3D('',#46175,#33229,#33230);
#26849=AXIS2_PLACEMENT_3D('',#46179,#33233,#33234);
#26850=AXIS2_PLACEMENT_3D('',#46180,#33235,#33236);
#26851=AXIS2_PLACEMENT_3D('',#46181,#33237,#33238);
#26852=AXIS2_PLACEMENT_3D('',#46190,#33243,#33244);
#26853=AXIS2_PLACEMENT_3D('',#46192,#33245,#33246);
#26854=AXIS2_PLACEMENT_3D('',#46194,#33248,#33249);
#26855=AXIS2_PLACEMENT_3D('',#46198,#33252,#33253);
#26856=AXIS2_PLACEMENT_3D('',#46199,#33254,#33255);
#26857=AXIS2_PLACEMENT_3D('',#46200,#33256,#33257);
#26858=AXIS2_PLACEMENT_3D('',#46209,#33262,#33263);
#26859=AXIS2_PLACEMENT_3D('',#46211,#33264,#33265);
#26860=AXIS2_PLACEMENT_3D('',#46213,#33267,#33268);
#26861=AXIS2_PLACEMENT_3D('',#46217,#33271,#33272);
#26862=AXIS2_PLACEMENT_3D('',#46218,#33273,#33274);
#26863=AXIS2_PLACEMENT_3D('',#46219,#33275,#33276);
#26864=AXIS2_PLACEMENT_3D('',#46228,#33281,#33282);
#26865=AXIS2_PLACEMENT_3D('',#46230,#33283,#33284);
#26866=AXIS2_PLACEMENT_3D('',#46232,#33286,#33287);
#26867=AXIS2_PLACEMENT_3D('',#46236,#33290,#33291);
#26868=AXIS2_PLACEMENT_3D('',#46237,#33292,#33293);
#26869=AXIS2_PLACEMENT_3D('',#46238,#33294,#33295);
#26870=AXIS2_PLACEMENT_3D('',#46247,#33300,#33301);
#26871=AXIS2_PLACEMENT_3D('',#46249,#33302,#33303);
#26872=AXIS2_PLACEMENT_3D('',#46251,#33305,#33306);
#26873=AXIS2_PLACEMENT_3D('',#46255,#33309,#33310);
#26874=AXIS2_PLACEMENT_3D('',#46256,#33311,#33312);
#26875=AXIS2_PLACEMENT_3D('',#46257,#33313,#33314);
#26876=AXIS2_PLACEMENT_3D('',#46266,#33319,#33320);
#26877=AXIS2_PLACEMENT_3D('',#46272,#33324,#33325);
#26878=AXIS2_PLACEMENT_3D('',#46278,#33329,#33330);
#26879=AXIS2_PLACEMENT_3D('',#46284,#33334,#33335);
#26880=AXIS2_PLACEMENT_3D('',#46290,#33339,#33340);
#26881=AXIS2_PLACEMENT_3D('',#46293,#33343,#33344);
#26882=AXIS2_PLACEMENT_3D('',#46294,#33345,#33346);
#26883=AXIS2_PLACEMENT_3D('',#46296,#33347,#33348);
#26884=AXIS2_PLACEMENT_3D('',#46297,#33349,#33350);
#26885=AXIS2_PLACEMENT_3D('',#46299,#33352,#33353);
#26886=AXIS2_PLACEMENT_3D('',#46300,#33354,#33355);
#26887=AXIS2_PLACEMENT_3D('',#46301,#33356,#33357);
#26888=AXIS2_PLACEMENT_3D('',#46303,#33358,#33359);
#26889=AXIS2_PLACEMENT_3D('',#46305,#33361,#33362);
#26890=AXIS2_PLACEMENT_3D('',#46307,#33363,#33364);
#26891=AXIS2_PLACEMENT_3D('',#46309,#33366,#33367);
#26892=AXIS2_PLACEMENT_3D('',#46311,#33368,#33369);
#26893=AXIS2_PLACEMENT_3D('',#46312,#33370,#33371);
#26894=AXIS2_PLACEMENT_3D('',#46314,#33372,#33373);
#26895=AXIS2_PLACEMENT_3D('',#46317,#33376,#33377);
#26896=AXIS2_PLACEMENT_3D('',#46319,#33378,#33379);
#26897=AXIS2_PLACEMENT_3D('',#46321,#33381,#33382);
#26898=AXIS2_PLACEMENT_3D('',#46322,#33383,#33384);
#26899=AXIS2_PLACEMENT_3D('',#46323,#33385,#33386);
#26900=AXIS2_PLACEMENT_3D('',#46325,#33387,#33388);
#26901=AXIS2_PLACEMENT_3D('',#46326,#33389,#33390);
#26902=AXIS2_PLACEMENT_3D('',#46328,#33391,#33392);
#26903=AXIS2_PLACEMENT_3D('',#46330,#33394,#33395);
#26904=AXIS2_PLACEMENT_3D('',#46332,#33396,#33397);
#26905=AXIS2_PLACEMENT_3D('',#46334,#33399,#33400);
#26906=AXIS2_PLACEMENT_3D('',#46336,#33401,#33402);
#26907=AXIS2_PLACEMENT_3D('',#46338,#33404,#33405);
#26908=AXIS2_PLACEMENT_3D('',#46339,#33406,#33407);
#26909=AXIS2_PLACEMENT_3D('',#46340,#33408,#33409);
#26910=AXIS2_PLACEMENT_3D('',#46341,#33410,#33411);
#26911=AXIS2_PLACEMENT_3D('',#46342,#33412,#33413);
#26912=AXIS2_PLACEMENT_3D('',#46343,#33414,#33415);
#26913=AXIS2_PLACEMENT_3D('',#46344,#33416,#33417);
#26914=AXIS2_PLACEMENT_3D('',#46345,#33418,#33419);
#26915=AXIS2_PLACEMENT_3D('',#46346,#33420,#33421);
#26916=AXIS2_PLACEMENT_3D('',#46347,#33422,#33423);
#26917=AXIS2_PLACEMENT_3D('',#46348,#33424,#33425);
#26918=AXIS2_PLACEMENT_3D('',#46349,#33426,#33427);
#26919=AXIS2_PLACEMENT_3D('',#46350,#33428,#33429);
#26920=AXIS2_PLACEMENT_3D('',#46351,#33430,#33431);
#26921=AXIS2_PLACEMENT_3D('',#46352,#33432,#33433);
#26922=AXIS2_PLACEMENT_3D('',#46353,#33434,#33435);
#26923=AXIS2_PLACEMENT_3D('',#46354,#33436,#33437);
#26924=AXIS2_PLACEMENT_3D('',#46355,#33438,#33439);
#26925=AXIS2_PLACEMENT_3D('',#46356,#33440,#33441);
#26926=AXIS2_PLACEMENT_3D('',#46357,#33442,#33443);
#26927=AXIS2_PLACEMENT_3D('',#46358,#33444,#33445);
#26928=AXIS2_PLACEMENT_3D('',#46359,#33446,#33447);
#26929=AXIS2_PLACEMENT_3D('',#46360,#33448,#33449);
#26930=AXIS2_PLACEMENT_3D('',#46361,#33450,#33451);
#26931=AXIS2_PLACEMENT_3D('',#46362,#33452,#33453);
#26932=AXIS2_PLACEMENT_3D('',#46363,#33454,#33455);
#26933=DIRECTION('axis',(0.,0.,1.));
#26934=DIRECTION('refdir',(1.,0.,0.));
#26935=DIRECTION('axis',(0.,0.,1.));
#26936=DIRECTION('refdir',(1.,0.,0.));
#26937=DIRECTION('center_axis',(0.,1.,0.));
#26938=DIRECTION('ref_axis',(1.,0.,0.));
#26939=DIRECTION('center_axis',(0.,1.,0.));
#26940=DIRECTION('ref_axis',(1.,0.,0.));
#26941=DIRECTION('',(-0.707106781186547,0.707106781186549,-8.65956056235492E-17));
#26942=DIRECTION('center_axis',(0.,-1.,0.));
#26943=DIRECTION('ref_axis',(1.,0.,0.));
#26944=DIRECTION('center_axis',(0.,1.,0.));
#26945=DIRECTION('ref_axis',(1.,0.,0.));
#26946=DIRECTION('center_axis',(0.,-1.,0.));
#26947=DIRECTION('ref_axis',(1.,0.,0.));
#26948=DIRECTION('center_axis',(0.,-1.,0.));
#26949=DIRECTION('ref_axis',(1.,0.,0.));
#26950=DIRECTION('',(0.,1.,0.));
#26951=DIRECTION('center_axis',(0.,1.,0.));
#26952=DIRECTION('ref_axis',(1.,0.,0.));
#26953=DIRECTION('center_axis',(0.,1.,0.));
#26954=DIRECTION('ref_axis',(1.,0.,0.));
#26955=DIRECTION('center_axis',(0.,1.,0.));
#26956=DIRECTION('ref_axis',(1.,0.,0.));
#26957=DIRECTION('',(-0.707106781186547,0.707106781186549,-8.65956056235492E-17));
#26958=DIRECTION('center_axis',(0.,-1.,0.));
#26959=DIRECTION('ref_axis',(1.,0.,0.));
#26960=DIRECTION('center_axis',(0.,1.,0.));
#26961=DIRECTION('ref_axis',(1.,0.,0.));
#26962=DIRECTION('center_axis',(0.,-1.,0.));
#26963=DIRECTION('ref_axis',(1.,0.,0.));
#26964=DIRECTION('center_axis',(0.,-1.,0.));
#26965=DIRECTION('ref_axis',(1.,0.,0.));
#26966=DIRECTION('',(0.,1.,0.));
#26967=DIRECTION('center_axis',(0.,1.,0.));
#26968=DIRECTION('ref_axis',(1.,0.,0.));
#26969=DIRECTION('center_axis',(0.,-1.,0.));
#26970=DIRECTION('ref_axis',(0.,0.,-1.));
#26971=DIRECTION('center_axis',(0.,-1.,0.));
#26972=DIRECTION('ref_axis',(0.,0.,-1.));
#26973=DIRECTION('',(8.65956056235494E-17,0.707106781186547,-0.707106781186548));
#26974=DIRECTION('center_axis',(0.,1.,0.));
#26975=DIRECTION('ref_axis',(0.,0.,-1.));
#26976=DIRECTION('center_axis',(0.,1.,0.));
#26977=DIRECTION('ref_axis',(0.,0.,-1.));
#26978=DIRECTION('center_axis',(0.,1.,0.));
#26979=DIRECTION('ref_axis',(0.,0.,1.));
#26980=DIRECTION('',(0.,1.,0.));
#26981=DIRECTION('center_axis',(0.,-1.,0.));
#26982=DIRECTION('ref_axis',(0.,0.,1.));
#26983=DIRECTION('center_axis',(0.,1.,0.));
#26984=DIRECTION('ref_axis',(0.,0.,1.));
#26985=DIRECTION('center_axis',(0.,1.,0.));
#26986=DIRECTION('ref_axis',(1.,0.,0.));
#26987=DIRECTION('center_axis',(0.,1.,0.));
#26988=DIRECTION('ref_axis',(0.,0.,1.));
#26989=DIRECTION('center_axis',(0.,1.,0.));
#26990=DIRECTION('ref_axis',(0.,0.,1.));
#26991=DIRECTION('',(8.65956056235493E-17,-0.707106781186548,0.707106781186548));
#26992=DIRECTION('center_axis',(0.,1.,0.));
#26993=DIRECTION('ref_axis',(1.,0.,0.));
#26994=DIRECTION('',(0.,0.,-1.));
#26995=DIRECTION('center_axis',(0.,-1.,0.));
#26996=DIRECTION('ref_axis',(-6.12323399573676E-17,0.,1.));
#26997=DIRECTION('',(0.,0.,1.));
#26998=DIRECTION('center_axis',(0.,-1.,0.));
#26999=DIRECTION('ref_axis',(8.54643792476272E-17,0.,-1.));
#27000=DIRECTION('',(-0.707106781186549,0.,0.707106781186546));
#27001=DIRECTION('',(0.707106781186551,0.,-0.707106781186544));
#27002=DIRECTION('center_axis',(-0.707106781186547,0.,-0.707106781186548));
#27003=DIRECTION('ref_axis',(-0.707106781186548,0.,0.707106781186547));
#27004=DIRECTION('',(-0.707106781186548,0.,0.707106781186547));
#27005=DIRECTION('',(0.,-1.,0.));
#27006=DIRECTION('',(0.,1.,0.));
#27007=DIRECTION('center_axis',(0.,1.,0.));
#27008=DIRECTION('ref_axis',(1.,0.,0.));
#27009=DIRECTION('',(1.,0.,0.));
#27010=DIRECTION('center_axis',(0.,1.,0.));
#27011=DIRECTION('ref_axis',(-0.707106781186547,0.,0.707106781186547));
#27012=DIRECTION('',(0.,0.,1.));
#27013=DIRECTION('center_axis',(0.,1.,0.));
#27014=DIRECTION('ref_axis',(-0.707106781186547,0.,-0.707106781186547));
#27015=DIRECTION('',(-1.,0.,0.));
#27016=DIRECTION('center_axis',(0.,1.,0.));
#27017=DIRECTION('ref_axis',(0.707106781186548,0.,-0.707106781186547));
#27018=DIRECTION('',(0.,0.,-1.));
#27019=DIRECTION('center_axis',(0.,1.,0.));
#27020=DIRECTION('ref_axis',(0.707106781186547,0.,0.707106781186548));
#27021=DIRECTION('',(1.,0.,0.));
#27022=DIRECTION('center_axis',(0.,1.,0.));
#27023=DIRECTION('ref_axis',(6.12323399573677E-17,0.,1.));
#27024=DIRECTION('center_axis',(0.,-1.,0.));
#27025=DIRECTION('ref_axis',(1.,0.,0.));
#27026=DIRECTION('',(-1.,0.,0.));
#27027=DIRECTION('',(-0.707106781186549,0.,-0.707106781186546));
#27028=DIRECTION('',(5.04646829375071E-17,0.,-1.));
#27029=DIRECTION('center_axis',(0.,1.,0.));
#27030=DIRECTION('ref_axis',(0.38268343236509,0.,-0.923879532511287));
#27031=DIRECTION('',(-0.707106781186548,0.,0.707106781186548));
#27032=DIRECTION('',(-0.707106781186548,0.,-0.707106781186548));
#27033=DIRECTION('',(0.707106781186548,0.,-0.707106781186548));
#27034=DIRECTION('center_axis',(0.,1.,0.));
#27035=DIRECTION('ref_axis',(0.892598706858255,0.,-0.450852025075824));
#27036=DIRECTION('center_axis',(0.,1.,0.));
#27037=DIRECTION('ref_axis',(-0.117423234417673,0.,-0.99308196238724));
#27038=DIRECTION('',(0.,0.,1.));
#27039=DIRECTION('center_axis',(0.,-1.,0.));
#27040=DIRECTION('ref_axis',(0.707106781186547,0.,-0.707106781186548));
#27041=DIRECTION('',(1.,0.,0.));
#27042=DIRECTION('center_axis',(0.,-1.,0.));
#27043=DIRECTION('ref_axis',(-0.707106781186548,0.,-0.707106781186548));
#27044=DIRECTION('',(0.,0.,-1.));
#27045=DIRECTION('center_axis',(0.,1.,0.));
#27046=DIRECTION('ref_axis',(0.12088535091488,0.,-0.992666475677599));
#27047=DIRECTION('center_axis',(0.,1.,0.));
#27048=DIRECTION('ref_axis',(-0.899687500253878,0.,-0.436534536877586));
#27049=DIRECTION('',(0.707106781186548,0.,0.707106781186547));
#27050=DIRECTION('',(8.91235409254052E-15,0.,1.));
#27051=DIRECTION('',(-0.707106781186548,0.,0.707106781186547));
#27052=DIRECTION('',(-1.,0.,-8.91235409254068E-15));
#27053=DIRECTION('',(-0.707106781186548,0.,-0.707106781186548));
#27054=DIRECTION('center_axis',(0.,1.,0.));
#27055=DIRECTION('ref_axis',(-0.367874908669274,0.,-0.929875288182008));
#27056=DIRECTION('',(-5.04646829375071E-17,0.,1.));
#27057=DIRECTION('center_axis',(0.,-1.,0.));
#27058=DIRECTION('ref_axis',(0.707106781186548,0.,0.707106781186547));
#27059=DIRECTION('',(0.,0.,1.));
#27060=DIRECTION('center_axis',(0.,1.,0.));
#27061=DIRECTION('ref_axis',(-0.117423234417673,0.,0.99308196238724));
#27062=DIRECTION('center_axis',(0.,1.,0.));
#27063=DIRECTION('ref_axis',(0.868290222566564,0.,0.496056538506759));
#27064=DIRECTION('',(-1.,0.,0.));
#27065=DIRECTION('center_axis',(0.,-1.,0.));
#27066=DIRECTION('ref_axis',(0.811029676142761,0.,0.585005012299696));
#27067=DIRECTION('center_axis',(0.,1.,0.));
#27068=DIRECTION('ref_axis',(0.,0.,1.));
#27069=DIRECTION('center_axis',(0.,1.,0.));
#27070=DIRECTION('ref_axis',(0.,0.,1.));
#27071=DIRECTION('center_axis',(0.,-1.,0.));
#27072=DIRECTION('ref_axis',(-0.811029676142761,0.,0.585005012299696));
#27073=DIRECTION('center_axis',(0.,1.,0.));
#27074=DIRECTION('ref_axis',(0.,0.,1.));
#27075=DIRECTION('center_axis',(0.,-1.,0.));
#27076=DIRECTION('ref_axis',(-0.707106781186547,0.,0.707106781186548));
#27077=DIRECTION('',(-1.,0.,0.));
#27078=DIRECTION('center_axis',(0.,1.,0.));
#27079=DIRECTION('ref_axis',(-0.868290222566564,0.,0.496056538506759));
#27080=DIRECTION('center_axis',(0.,1.,0.));
#27081=DIRECTION('ref_axis',(0.117423234417673,0.,0.99308196238724));
#27082=DIRECTION('',(0.,0.,-1.));
#27083=DIRECTION('center_axis',(0.,-1.,0.));
#27084=DIRECTION('ref_axis',(1.,0.,0.));
#27085=DIRECTION('center_axis',(1.,0.,0.));
#27086=DIRECTION('ref_axis',(0.,-0.707106781186547,-0.707106781186548));
#27087=DIRECTION('',(1.,0.,0.));
#27088=DIRECTION('center_axis',(0.,0.,-1.));
#27089=DIRECTION('ref_axis',(1.,0.,0.));
#27090=DIRECTION('',(-1.,0.,0.));
#27091=DIRECTION('',(0.,1.,0.));
#27092=DIRECTION('',(0.707106781186548,0.,0.707106781186547));
#27093=DIRECTION('center_axis',(0.707106781186553,0.,-0.707106781186542));
#27094=DIRECTION('ref_axis',(-0.707106781186542,0.,-0.707106781186553));
#27095=DIRECTION('',(-0.707106781186542,0.,-0.707106781186553));
#27096=DIRECTION('',(0.,-1.,0.));
#27097=DIRECTION('center_axis',(-5.04646829375071E-17,0.,1.));
#27098=DIRECTION('ref_axis',(0.707106781186548,-0.707106781186548,0.));
#27099=DIRECTION('',(-5.04646829375071E-17,0.,1.));
#27100=DIRECTION('center_axis',(1.,0.,5.04646829375071E-17));
#27101=DIRECTION('ref_axis',(-5.04646829375071E-17,0.,1.));
#27102=DIRECTION('',(5.04646829375071E-17,0.,-1.));
#27103=DIRECTION('',(0.,1.,0.));
#27104=DIRECTION('center_axis',(0.,-1.,0.));
#27105=DIRECTION('ref_axis',(1.,0.,0.));
#27106=DIRECTION('',(0.707106781186546,0.707106781186549,8.65956056235491E-17));
#27107=DIRECTION('center_axis',(0.,1.,0.));
#27108=DIRECTION('ref_axis',(1.,0.,0.));
#27109=DIRECTION('center_axis',(0.,-1.,0.));
#27110=DIRECTION('ref_axis',(1.,0.,0.));
#27111=DIRECTION('center_axis',(0.,-1.,0.));
#27112=DIRECTION('ref_axis',(1.,0.,0.));
#27113=DIRECTION('',(0.,-1.,0.));
#27114=DIRECTION('center_axis',(0.,-1.,0.));
#27115=DIRECTION('ref_axis',(1.,0.,0.));
#27116=DIRECTION('',(0.707106781186546,0.707106781186549,8.65956056235491E-17));
#27117=DIRECTION('center_axis',(0.,1.,0.));
#27118=DIRECTION('ref_axis',(1.,0.,0.));
#27119=DIRECTION('center_axis',(0.,-1.,0.));
#27120=DIRECTION('ref_axis',(1.,0.,0.));
#27121=DIRECTION('center_axis',(0.,-1.,0.));
#27122=DIRECTION('ref_axis',(1.,0.,0.));
#27123=DIRECTION('',(0.,-1.,0.));
#27124=DIRECTION('center_axis',(-0.15189042169011,0.,0.988397339028592));
#27125=DIRECTION('ref_axis',(0.988397339028592,0.,0.15189042169011));
#27126=DIRECTION('',(0.,-1.,0.));
#27127=DIRECTION('',(0.,1.,0.));
#27128=DIRECTION('center_axis',(0.,-1.,0.));
#27129=DIRECTION('ref_axis',(1.,0.,0.));
#27130=DIRECTION('center_axis',(0.,-1.,0.));
#27131=DIRECTION('ref_axis',(1.,0.,0.));
#27132=DIRECTION('',(0.,-1.,0.));
#27133=DIRECTION('center_axis',(0.,-1.,0.));
#27134=DIRECTION('ref_axis',(1.,0.,0.));
#27135=DIRECTION('center_axis',(0.,1.,0.));
#27136=DIRECTION('ref_axis',(0.811029676142761,0.,0.585005012299696));
#27137=DIRECTION('',(0.,1.,0.));
#27138=DIRECTION('center_axis',(0.,-1.,0.));
#27139=DIRECTION('ref_axis',(1.,0.,0.));
#27140=DIRECTION('center_axis',(0.15189042169011,0.,0.988397339028592));
#27141=DIRECTION('ref_axis',(0.988397339028592,0.,-0.15189042169011));
#27142=DIRECTION('',(0.,1.,0.));
#27143=DIRECTION('',(0.,-1.,0.));
#27144=DIRECTION('center_axis',(0.,-1.,0.));
#27145=DIRECTION('ref_axis',(1.,0.,0.));
#27146=DIRECTION('center_axis',(0.,-1.,0.));
#27147=DIRECTION('ref_axis',(1.,0.,0.));
#27148=DIRECTION('',(0.,-1.,0.));
#27149=DIRECTION('center_axis',(0.,1.,0.));
#27150=DIRECTION('ref_axis',(-0.811029676142761,0.,0.585005012299696));
#27151=DIRECTION('center_axis',(0.,-1.,0.));
#27152=DIRECTION('ref_axis',(1.,0.,0.));
#27153=DIRECTION('',(0.,-1.,0.));
#27154=DIRECTION('center_axis',(0.,1.,0.));
#27155=DIRECTION('ref_axis',(-0.811029676142761,0.,0.585005012299696));
#27156=DIRECTION('center_axis',(-0.889975696162041,0.,-0.456007960720962));
#27157=DIRECTION('ref_axis',(-0.456007960720962,0.,0.889975696162041));
#27158=DIRECTION('',(0.,1.,0.));
#27159=DIRECTION('center_axis',(0.889975696162041,0.,-0.456007960720962));
#27160=DIRECTION('ref_axis',(-0.456007960720962,0.,-0.889975696162041));
#27161=DIRECTION('',(0.,-1.,0.));
#27162=DIRECTION('center_axis',(0.,1.,0.));
#27163=DIRECTION('ref_axis',(1.,0.,0.));
#27164=DIRECTION('center_axis',(0.,1.,0.));
#27165=DIRECTION('ref_axis',(1.,0.,0.));
#27166=DIRECTION('',(0.707106781186546,-0.707106781186549,-8.65956056235491E-17));
#27167=DIRECTION('center_axis',(0.,1.,0.));
#27168=DIRECTION('ref_axis',(1.,0.,0.));
#27169=DIRECTION('center_axis',(0.,-1.,0.));
#27170=DIRECTION('ref_axis',(0.707106781186548,0.,-0.707106781186547));
#27171=DIRECTION('',(1.,0.,0.));
#27172=DIRECTION('center_axis',(0.,-1.,0.));
#27173=DIRECTION('ref_axis',(-0.707106781186547,0.,-0.707106781186547));
#27174=DIRECTION('',(0.,0.,-1.));
#27175=DIRECTION('center_axis',(0.,-1.,0.));
#27176=DIRECTION('ref_axis',(-0.707106781186547,0.,0.707106781186547));
#27177=DIRECTION('',(-1.,0.,0.));
#27178=DIRECTION('center_axis',(0.,-1.,0.));
#27179=DIRECTION('ref_axis',(0.707106781186547,0.,0.707106781186548));
#27180=DIRECTION('',(0.,0.,1.));
#27181=DIRECTION('center_axis',(0.,1.,0.));
#27182=DIRECTION('ref_axis',(1.,0.,0.));
#27183=DIRECTION('center_axis',(0.,1.,0.));
#27184=DIRECTION('ref_axis',(1.,0.,0.));
#27185=DIRECTION('center_axis',(0.,1.,0.));
#27186=DIRECTION('ref_axis',(1.,0.,0.));
#27187=DIRECTION('',(0.,0.,-1.));
#27188=DIRECTION('center_axis',(0.,1.,0.));
#27189=DIRECTION('ref_axis',(-6.12323399573676E-17,0.,1.));
#27190=DIRECTION('',(0.,0.,1.));
#27191=DIRECTION('center_axis',(0.,1.,0.));
#27192=DIRECTION('ref_axis',(6.12323399573676E-17,0.,-1.));
#27193=DIRECTION('center_axis',(0.,-1.,0.));
#27194=DIRECTION('ref_axis',(1.,0.,0.));
#27195=DIRECTION('center_axis',(0.,-1.,0.));
#27196=DIRECTION('ref_axis',(1.,0.,0.));
#27197=DIRECTION('center_axis',(0.,1.,0.));
#27198=DIRECTION('ref_axis',(1.,0.,0.));
#27199=DIRECTION('center_axis',(0.,1.,0.));
#27200=DIRECTION('ref_axis',(1.,0.,0.));
#27201=DIRECTION('center_axis',(0.,1.,0.));
#27202=DIRECTION('ref_axis',(1.,0.,0.));
#27203=DIRECTION('',(0.707106781186546,-0.707106781186549,-8.65956056235491E-17));
#27204=DIRECTION('center_axis',(0.,1.,0.));
#27205=DIRECTION('ref_axis',(1.,0.,0.));
#27206=DIRECTION('',(0.707106781186546,-0.707106781186549,-8.65956056235491E-17));
#27207=DIRECTION('center_axis',(0.,1.,0.));
#27208=DIRECTION('ref_axis',(1.,0.,0.));
#27209=DIRECTION('',(0.707106781186546,-0.707106781186549,-8.65956056235491E-17));
#27210=DIRECTION('center_axis',(0.,1.,0.));
#27211=DIRECTION('ref_axis',(1.,0.,0.));
#27212=DIRECTION('',(0.707106781186546,-0.707106781186549,-8.65956056235491E-17));
#27213=DIRECTION('center_axis',(0.,-1.,0.));
#27214=DIRECTION('ref_axis',(1.,0.,0.));
#27215=DIRECTION('center_axis',(0.,1.,0.));
#27216=DIRECTION('ref_axis',(1.,0.,0.));
#27217=DIRECTION('center_axis',(0.,1.,0.));
#27218=DIRECTION('ref_axis',(1.,0.,0.));
#27219=DIRECTION('',(0.,1.,0.));
#27220=DIRECTION('center_axis',(0.,1.,0.));
#27221=DIRECTION('ref_axis',(1.,0.,0.));
#27222=DIRECTION('',(0.707106781186546,-0.707106781186549,-8.65956056235491E-17));
#27223=DIRECTION('center_axis',(0.,-1.,0.));
#27224=DIRECTION('ref_axis',(1.,0.,0.));
#27225=DIRECTION('center_axis',(0.,1.,0.));
#27226=DIRECTION('ref_axis',(1.,0.,0.));
#27227=DIRECTION('center_axis',(0.,1.,0.));
#27228=DIRECTION('ref_axis',(1.,0.,0.));
#27229=DIRECTION('',(0.,1.,0.));
#27230=DIRECTION('',(-1.25607396694705E-14,2.74766180269668E-15,-1.));
#27231=DIRECTION('center_axis',(-1.,0.,0.));
#27232=DIRECTION('ref_axis',(0.,0.,1.));
#27233=DIRECTION('',(0.,0.,1.));
#27234=DIRECTION('',(0.,-1.,0.));
#27235=DIRECTION('',(0.,1.,0.));
#27236=DIRECTION('center_axis',(0.707106781186548,0.,-0.707106781186547));
#27237=DIRECTION('ref_axis',(-0.5,-0.707106781186548,-0.5));
#27238=DIRECTION('',(0.707106781186548,0.,-0.707106781186547));
#27239=DIRECTION('center_axis',(-0.707106781186547,0.,-0.707106781186548));
#27240=DIRECTION('ref_axis',(0.707106781186548,0.,-0.707106781186547));
#27241=DIRECTION('',(-0.707106781186548,0.,0.707106781186547));
#27242=DIRECTION('',(0.,1.,0.));
#27243=DIRECTION('',(1.,0.,-1.25607396694702E-14));
#27244=DIRECTION('center_axis',(0.,0.,-1.));
#27245=DIRECTION('ref_axis',(-1.,0.,0.));
#27246=DIRECTION('',(-1.,0.,0.));
#27247=DIRECTION('',(0.,-1.,0.));
#27248=DIRECTION('center_axis',(0.707106781186548,0.,0.707106781186548));
#27249=DIRECTION('ref_axis',(0.5,-0.707106781186548,-0.5));
#27250=DIRECTION('',(0.707106781186548,0.,0.707106781186548));
#27251=DIRECTION('center_axis',(0.707106781186548,0.,-0.707106781186548));
#27252=DIRECTION('ref_axis',(0.707106781186548,0.,0.707106781186548));
#27253=DIRECTION('',(-0.707106781186548,0.,-0.707106781186548));
#27254=DIRECTION('',(0.,1.,0.));
#27255=DIRECTION('center_axis',(0.,-1.,0.));
#27256=DIRECTION('ref_axis',(1.,0.,0.));
#27257=DIRECTION('',(0.707106781186546,0.707106781186549,8.65956056235492E-17));
#27258=DIRECTION('center_axis',(0.,-1.,0.));
#27259=DIRECTION('ref_axis',(1.,0.,0.));
#27260=DIRECTION('',(0.707106781186546,0.707106781186549,8.65956056235492E-17));
#27261=DIRECTION('center_axis',(0.,0.,-1.));
#27262=DIRECTION('ref_axis',(-1.,0.,0.));
#27263=DIRECTION('',(-1.,0.,0.));
#27264=DIRECTION('',(0.,-1.,0.));
#27265=DIRECTION('',(-1.,0.,0.));
#27266=DIRECTION('',(0.,1.,0.));
#27267=DIRECTION('center_axis',(-0.707106781186548,0.,0.707106781186548));
#27268=DIRECTION('ref_axis',(-0.5,-0.707106781186546,-0.500000000000002));
#27269=DIRECTION('',(-0.499999999999991,-0.707106781186561,0.499999999999991));
#27270=DIRECTION('center_axis',(0.707106781186548,0.,-0.707106781186548));
#27271=DIRECTION('ref_axis',(-0.5,-0.707106781186546,-0.500000000000002));
#27272=DIRECTION('center_axis',(-0.707106781186548,0.,0.707106781186548));
#27273=DIRECTION('ref_axis',(-0.500000000000001,-0.707106781186546,-0.500000000000001));
#27274=DIRECTION('center_axis',(0.5,-0.707106781186547,-0.5));
#27275=DIRECTION('ref_axis',(-0.707106781186548,0.,-0.707106781186548));
#27276=DIRECTION('',(-0.5,-0.707106781186548,0.5));
#27277=DIRECTION('',(0.707106781186548,0.,0.707106781186548));
#27278=DIRECTION('center_axis',(-0.707106781186548,0.,0.707106781186548));
#27279=DIRECTION('ref_axis',(0.499999999999999,-0.707106781186548,0.499999999999999));
#27280=DIRECTION('',(0.,-3.92523114670944E-16,1.));
#27281=DIRECTION('center_axis',(0.707106781186548,0.,-0.707106781186548));
#27282=DIRECTION('ref_axis',(0.5,-0.707106781186548,0.5));
#27283=DIRECTION('center_axis',(-0.707106781186548,0.,0.707106781186548));
#27284=DIRECTION('ref_axis',(0.5,-0.707106781186548,0.5));
#27285=DIRECTION('center_axis',(1.,0.,0.));
#27286=DIRECTION('ref_axis',(0.,0.,-1.));
#27287=DIRECTION('',(0.,0.,-1.));
#27288=DIRECTION('',(0.,-1.,0.));
#27289=DIRECTION('',(0.,1.,0.));
#27290=DIRECTION('center_axis',(0.707106781186548,0.,-0.707106781186548));
#27291=DIRECTION('ref_axis',(0.707106781186548,0.,0.707106781186548));
#27292=DIRECTION('',(-0.707106781186548,0.,-0.707106781186548));
#27293=DIRECTION('center_axis',(0.,1.,0.));
#27294=DIRECTION('ref_axis',(0.,0.,1.));
#27295=DIRECTION('center_axis',(0.,1.,0.));
#27296=DIRECTION('ref_axis',(6.12323399573677E-17,0.,1.));
#27297=DIRECTION('center_axis',(0.,-1.,0.));
#27298=DIRECTION('ref_axis',(6.12323399573677E-17,0.,1.));
#27299=DIRECTION('center_axis',(0.,-1.,0.));
#27300=DIRECTION('ref_axis',(1.,0.,0.));
#27301=DIRECTION('',(0.,1.,0.));
#27302=DIRECTION('center_axis',(0.,-1.,0.));
#27303=DIRECTION('ref_axis',(6.12323399573677E-17,0.,1.));
#27304=DIRECTION('',(0.,-1.,0.));
#27305=DIRECTION('center_axis',(0.,-1.,0.));
#27306=DIRECTION('ref_axis',(0.136763231432696,0.,0.990603764644617));
#27307=DIRECTION('center_axis',(0.,-1.,0.));
#27308=DIRECTION('ref_axis',(0.117423234417673,0.,0.99308196238724));
#27309=DIRECTION('center_axis',(0.,-1.,0.));
#27310=DIRECTION('ref_axis',(0.,0.,-1.));
#27311=DIRECTION('center_axis',(0.,-1.,0.));
#27312=DIRECTION('ref_axis',(-0.868290222566564,0.,0.496056538506759));
#27313=DIRECTION('center_axis',(0.,1.,0.));
#27314=DIRECTION('ref_axis',(0.,0.,1.));
#27315=DIRECTION('center_axis',(-1.48029736616687E-15,0.,1.));
#27316=DIRECTION('ref_axis',(0.,-1.,0.));
#27317=DIRECTION('center_axis',(0.,1.,0.));
#27318=DIRECTION('ref_axis',(-0.707106781186547,0.,0.707106781186548));
#27319=DIRECTION('center_axis',(-1.,0.,0.));
#27320=DIRECTION('ref_axis',(0.,0.,-1.));
#27321=DIRECTION('center_axis',(1.,0.,0.));
#27322=DIRECTION('ref_axis',(0.,-0.707106781186549,-0.707106781186546));
#27323=DIRECTION('',(1.,0.,0.));
#27324=DIRECTION('center_axis',(0.,0.,1.));
#27325=DIRECTION('ref_axis',(0.707106781186548,-0.707106781186547,0.));
#27326=DIRECTION('',(0.,0.,1.));
#27327=DIRECTION('center_axis',(0.,-1.,0.));
#27328=DIRECTION('ref_axis',(1.,0.,0.));
#27329=DIRECTION('',(0.,-1.,0.));
#27330=DIRECTION('center_axis',(0.,1.,0.));
#27331=DIRECTION('ref_axis',(1.,0.,0.));
#27332=DIRECTION('',(0.,-1.,0.));
#27333=DIRECTION('center_axis',(0.,0.,1.));
#27334=DIRECTION('ref_axis',(1.,0.,0.));
#27335=DIRECTION('',(0.,1.,0.));
#27336=DIRECTION('',(1.,0.,0.));
#27337=DIRECTION('center_axis',(0.,1.,0.));
#27338=DIRECTION('ref_axis',(-1.,0.,-1.00929365875014E-16));
#27339=DIRECTION('',(0.,1.,0.));
#27340=DIRECTION('center_axis',(0.,1.,0.));
#27341=DIRECTION('ref_axis',(-1.,0.,-1.00929365875014E-16));
#27342=DIRECTION('center_axis',(0.,-1.,0.));
#27343=DIRECTION('ref_axis',(0.,0.,-1.));
#27344=DIRECTION('center_axis',(0.,-1.,0.));
#27345=DIRECTION('ref_axis',(0.868290222566564,0.,0.496056538506759));
#27346=DIRECTION('center_axis',(0.,-1.,0.));
#27347=DIRECTION('ref_axis',(-0.136763231432696,0.,0.990603764644617));
#27348=DIRECTION('center_axis',(0.,-1.,0.));
#27349=DIRECTION('ref_axis',(-0.117423234417673,0.,0.99308196238724));
#27350=DIRECTION('center_axis',(0.,1.,0.));
#27351=DIRECTION('ref_axis',(0.,0.,1.));
#27352=DIRECTION('center_axis',(1.,0.,2.96059473233376E-15));
#27353=DIRECTION('ref_axis',(0.,-1.,0.));
#27354=DIRECTION('center_axis',(0.,1.,0.));
#27355=DIRECTION('ref_axis',(0.707106781186548,0.,0.707106781186547));
#27356=DIRECTION('center_axis',(0.,0.,1.));
#27357=DIRECTION('ref_axis',(-1.,0.,0.));
#27358=DIRECTION('center_axis',(0.,0.,-1.));
#27359=DIRECTION('ref_axis',(-0.707106781186548,-0.707106781186547,0.));
#27360=DIRECTION('',(0.,0.,-1.));
#27361=DIRECTION('center_axis',(1.,0.,0.));
#27362=DIRECTION('ref_axis',(0.,-0.707106781186549,-0.707106781186546));
#27363=DIRECTION('',(1.,0.,0.));
#27364=DIRECTION('center_axis',(0.,-1.,0.));
#27365=DIRECTION('ref_axis',(1.,0.,0.));
#27366=DIRECTION('',(0.,-1.,0.));
#27367=DIRECTION('center_axis',(0.,1.,0.));
#27368=DIRECTION('ref_axis',(1.,0.,0.));
#27369=DIRECTION('',(0.,-1.,0.));
#27370=DIRECTION('center_axis',(1.,0.,0.));
#27371=DIRECTION('ref_axis',(0.,0.,-1.));
#27372=DIRECTION('',(0.,1.,0.));
#27373=DIRECTION('',(0.,0.,-1.));
#27374=DIRECTION('center_axis',(0.,1.,0.));
#27375=DIRECTION('ref_axis',(2.01858731750029E-16,0.,1.));
#27376=DIRECTION('',(0.,1.,0.));
#27377=DIRECTION('center_axis',(0.,1.,0.));
#27378=DIRECTION('ref_axis',(2.01858731750029E-16,0.,1.));
#27379=DIRECTION('center_axis',(0.,-1.,0.));
#27380=DIRECTION('ref_axis',(1.22464679914735E-16,0.,1.));
#27381=DIRECTION('center_axis',(0.,-1.,0.));
#27382=DIRECTION('ref_axis',(0.,0.,-1.));
#27383=DIRECTION('center_axis',(0.,-1.,0.));
#27384=DIRECTION('ref_axis',(0.38268343236509,0.,-0.923879532511287));
#27385=DIRECTION('center_axis',(0.,-1.,0.));
#27386=DIRECTION('ref_axis',(1.,0.,0.));
#27387=DIRECTION('center_axis',(0.,1.,0.));
#27388=DIRECTION('ref_axis',(1.,0.,0.));
#27389=DIRECTION('',(0.,-1.,0.));
#27390=DIRECTION('center_axis',(0.,-1.,0.));
#27391=DIRECTION('ref_axis',(0.,0.,-1.));
#27392=DIRECTION('center_axis',(0.,-1.,0.));
#27393=DIRECTION('ref_axis',(0.12088535091488,0.,-0.992666475677599));
#27394=DIRECTION('center_axis',(0.,-1.,0.));
#27395=DIRECTION('ref_axis',(1.,0.,0.));
#27396=DIRECTION('',(0.,-1.,0.));
#27397=DIRECTION('center_axis',(0.,1.,0.));
#27398=DIRECTION('ref_axis',(1.,0.,0.));
#27399=DIRECTION('',(0.,-1.,0.));
#27400=DIRECTION('center_axis',(0.,0.,-1.));
#27401=DIRECTION('ref_axis',(-0.707106781186548,-0.707106781186547,0.));
#27402=DIRECTION('',(0.,0.,-1.));
#27403=DIRECTION('center_axis',(0.,0.,1.));
#27404=DIRECTION('ref_axis',(-1.,0.,0.));
#27405=DIRECTION('center_axis',(0.,-1.,0.));
#27406=DIRECTION('ref_axis',(0.,0.,-1.));
#27407=DIRECTION('center_axis',(0.,-1.,0.));
#27408=DIRECTION('ref_axis',(-0.117423234417673,0.,-0.99308196238724));
#27409=DIRECTION('center_axis',(0.,-1.,0.));
#27410=DIRECTION('ref_axis',(0.,0.,-1.));
#27411=DIRECTION('center_axis',(0.,-1.,0.));
#27412=DIRECTION('ref_axis',(0.892598706858255,0.,-0.450852025075824));
#27413=DIRECTION('center_axis',(0.,1.,0.));
#27414=DIRECTION('ref_axis',(0.,0.,1.));
#27415=DIRECTION('center_axis',(1.,0.,-2.96059473233378E-15));
#27416=DIRECTION('ref_axis',(2.96059473233378E-15,0.,1.));
#27417=DIRECTION('center_axis',(0.,1.,0.));
#27418=DIRECTION('ref_axis',(0.707106781186547,0.,-0.707106781186548));
#27419=DIRECTION('center_axis',(-1.,0.,0.));
#27420=DIRECTION('ref_axis',(0.,-0.707106781186547,0.707106781186548));
#27421=DIRECTION('center_axis',(1.,0.,-2.96059473233374E-15));
#27422=DIRECTION('ref_axis',(2.96059473233374E-15,0.,1.));
#27423=DIRECTION('',(-1.,0.,0.));
#27424=DIRECTION('center_axis',(0.,1.,0.));
#27425=DIRECTION('ref_axis',(0.,0.,1.));
#27426=DIRECTION('center_axis',(0.,0.,-1.));
#27427=DIRECTION('ref_axis',(1.,0.,0.));
#27428=DIRECTION('center_axis',(0.,1.,0.));
#27429=DIRECTION('ref_axis',(-0.707106781186547,0.,-0.707106781186547));
#27430=DIRECTION('center_axis',(0.,0.,1.));
#27431=DIRECTION('ref_axis',(0.707106781186548,-0.707106781186547,0.));
#27432=DIRECTION('',(0.,0.,1.));
#27433=DIRECTION('center_axis',(-1.,0.,0.));
#27434=DIRECTION('ref_axis',(0.,0.,1.));
#27435=DIRECTION('',(0.,1.,0.));
#27436=DIRECTION('',(0.,0.,1.));
#27437=DIRECTION('center_axis',(0.,1.,0.));
#27438=DIRECTION('ref_axis',(2.01858731750029E-16,0.,-1.));
#27439=DIRECTION('',(0.,1.,0.));
#27440=DIRECTION('center_axis',(0.,1.,0.));
#27441=DIRECTION('ref_axis',(2.01858731750029E-16,0.,-1.));
#27442=DIRECTION('center_axis',(0.,0.,-1.));
#27443=DIRECTION('ref_axis',(-1.,0.,0.));
#27444=DIRECTION('',(0.,1.,0.));
#27445=DIRECTION('',(-1.,0.,0.));
#27446=DIRECTION('center_axis',(0.,1.,0.));
#27447=DIRECTION('ref_axis',(1.,0.,8.07434927000114E-16));
#27448=DIRECTION('',(0.,1.,0.));
#27449=DIRECTION('center_axis',(0.,1.,0.));
#27450=DIRECTION('ref_axis',(1.,0.,8.07434927000114E-16));
#27451=DIRECTION('center_axis',(1.,0.,0.));
#27452=DIRECTION('ref_axis',(0.,0.,-1.));
#27453=DIRECTION('',(0.,1.,0.));
#27454=DIRECTION('',(0.,0.,-1.));
#27455=DIRECTION('center_axis',(0.,-1.,0.));
#27456=DIRECTION('ref_axis',(1.,0.,0.));
#27457=DIRECTION('',(0.,-1.,0.));
#27458=DIRECTION('center_axis',(0.,1.,0.));
#27459=DIRECTION('ref_axis',(1.,0.,0.));
#27460=DIRECTION('center_axis',(0.,-1.,0.));
#27461=DIRECTION('ref_axis',(1.,0.,0.));
#27462=DIRECTION('',(0.,1.,0.));
#27463=DIRECTION('center_axis',(0.,1.,0.));
#27464=DIRECTION('ref_axis',(1.,0.,0.));
#27465=DIRECTION('center_axis',(0.,0.,-1.));
#27466=DIRECTION('ref_axis',(-0.707106781186548,-0.707106781186547,0.));
#27467=DIRECTION('center_axis',(-1.48029736616687E-15,0.,-1.));
#27468=DIRECTION('ref_axis',(0.,-1.,0.));
#27469=DIRECTION('',(0.,0.,-1.));
#27470=DIRECTION('center_axis',(0.,0.,1.));
#27471=DIRECTION('ref_axis',(-1.,0.,0.));
#27472=DIRECTION('center_axis',(0.,1.,0.));
#27473=DIRECTION('ref_axis',(0.,0.,1.));
#27474=DIRECTION('center_axis',(-1.,0.,0.));
#27475=DIRECTION('ref_axis',(0.,0.,-1.));
#27476=DIRECTION('center_axis',(0.,-1.,0.));
#27477=DIRECTION('ref_axis',(-0.707106781186548,0.,-0.707106781186548));
#27478=DIRECTION('center_axis',(1.,0.,0.));
#27479=DIRECTION('ref_axis',(0.,-0.707106781186547,-0.707106781186548));
#27480=DIRECTION('center_axis',(-1.,0.,0.));
#27481=DIRECTION('ref_axis',(0.,0.,-1.));
#27482=DIRECTION('',(1.,0.,0.));
#27483=DIRECTION('center_axis',(0.,1.,0.));
#27484=DIRECTION('ref_axis',(0.,0.,1.));
#27485=DIRECTION('center_axis',(0.,0.,-1.));
#27486=DIRECTION('ref_axis',(1.,0.,0.));
#27487=DIRECTION('center_axis',(0.,-1.,0.));
#27488=DIRECTION('ref_axis',(0.707106781186548,0.,-0.707106781186547));
#27489=DIRECTION('center_axis',(0.,0.,1.));
#27490=DIRECTION('ref_axis',(0.707106781186548,-0.707106781186547,0.));
#27491=DIRECTION('center_axis',(0.,0.,-1.));
#27492=DIRECTION('ref_axis',(1.,0.,0.));
#27493=DIRECTION('',(0.,0.,1.));
#27494=DIRECTION('center_axis',(0.,1.,0.));
#27495=DIRECTION('ref_axis',(0.,0.,1.));
#27496=DIRECTION('center_axis',(1.,0.,-5.92118946466749E-15));
#27497=DIRECTION('ref_axis',(5.92118946466749E-15,0.,1.));
#27498=DIRECTION('center_axis',(0.,-1.,0.));
#27499=DIRECTION('ref_axis',(0.707106781186547,0.,0.707106781186548));
#27500=DIRECTION('center_axis',(-1.,0.,0.));
#27501=DIRECTION('ref_axis',(0.,-0.707106781186547,0.707106781186548));
#27502=DIRECTION('',(-1.,0.,0.));
#27503=DIRECTION('center_axis',(0.,1.,0.));
#27504=DIRECTION('ref_axis',(0.,0.,1.));
#27505=DIRECTION('center_axis',(-1.,0.,0.));
#27506=DIRECTION('ref_axis',(0.,-1.,0.));
#27507=DIRECTION('center_axis',(0.,-1.,0.));
#27508=DIRECTION('ref_axis',(-0.707106781186548,0.,0.707106781186548));
#27509=DIRECTION('center_axis',(-1.,0.,0.));
#27510=DIRECTION('ref_axis',(0.,-0.707106781186547,0.707106781186548));
#27511=DIRECTION('',(-1.,0.,0.));
#27512=DIRECTION('center_axis',(0.,1.,0.));
#27513=DIRECTION('ref_axis',(1.,0.,0.));
#27514=DIRECTION('',(0.,1.,0.));
#27515=DIRECTION('center_axis',(0.,1.,0.));
#27516=DIRECTION('ref_axis',(0.707106781186548,0.,-0.707106781186547));
#27517=DIRECTION('',(0.,1.,0.));
#27518=DIRECTION('center_axis',(0.,0.,-1.));
#27519=DIRECTION('ref_axis',(-1.,0.,0.));
#27520=DIRECTION('',(0.,1.,0.));
#27521=DIRECTION('',(-1.,0.,0.));
#27522=DIRECTION('center_axis',(0.,1.,0.));
#27523=DIRECTION('ref_axis',(-3.1720657846433E-16,0.,-1.));
#27524=DIRECTION('',(0.,1.,0.));
#27525=DIRECTION('center_axis',(0.,1.,0.));
#27526=DIRECTION('ref_axis',(-0.707106781186548,0.,-0.707106781186548));
#27527=DIRECTION('center_axis',(-1.,0.,0.));
#27528=DIRECTION('ref_axis',(0.,0.,1.));
#27529=DIRECTION('',(0.,1.,0.));
#27530=DIRECTION('',(0.,0.,1.));
#27531=DIRECTION('center_axis',(0.,1.,0.));
#27532=DIRECTION('ref_axis',(-1.,0.,3.96508223080413E-16));
#27533=DIRECTION('',(0.,1.,0.));
#27534=DIRECTION('center_axis',(0.,1.,0.));
#27535=DIRECTION('ref_axis',(-0.707106781186548,0.,0.707106781186548));
#27536=DIRECTION('center_axis',(-0.707106781186548,0.,0.707106781186548));
#27537=DIRECTION('ref_axis',(0.5,-0.707106781186548,0.5));
#27538=DIRECTION('',(-0.707106781186548,0.,0.707106781186548));
#27539=DIRECTION('center_axis',(0.707106781186548,0.,0.707106781186548));
#27540=DIRECTION('ref_axis',(-0.707106781186548,0.,0.707106781186548));
#27541=DIRECTION('',(0.707106781186548,0.,-0.707106781186548));
#27542=DIRECTION('center_axis',(0.707106781186548,0.,-0.707106781186548));
#27543=DIRECTION('ref_axis',(-0.5,-0.707106781186546,-0.500000000000002));
#27544=DIRECTION('',(0.707106781186548,0.,-0.707106781186548));
#27545=DIRECTION('center_axis',(-0.707106781186548,0.,-0.707106781186548));
#27546=DIRECTION('ref_axis',(0.707106781186548,0.,-0.707106781186548));
#27547=DIRECTION('',(-0.707106781186548,0.,0.707106781186548));
#27548=DIRECTION('center_axis',(0.,-1.,0.));
#27549=DIRECTION('ref_axis',(0.,0.,-1.));
#27550=DIRECTION('center_axis',(0.,-1.,0.));
#27551=DIRECTION('ref_axis',(-0.367874908669274,0.,-0.929875288182008));
#27552=DIRECTION('center_axis',(-0.707106781186548,0.,-0.707106781186547));
#27553=DIRECTION('ref_axis',(-0.499999999999999,-0.707106781186548,0.500000000000001));
#27554=DIRECTION('',(-0.707106781186548,0.,-0.707106781186547));
#27555=DIRECTION('center_axis',(0.,-1.,0.));
#27556=DIRECTION('ref_axis',(0.,0.,-1.));
#27557=DIRECTION('center_axis',(0.,-1.,0.));
#27558=DIRECTION('ref_axis',(-0.899687500253878,0.,-0.436534536877586));
#27559=DIRECTION('center_axis',(0.,-1.,0.));
#27560=DIRECTION('ref_axis',(1.,0.,0.));
#27561=DIRECTION('center_axis',(0.,1.,0.));
#27562=DIRECTION('ref_axis',(1.,0.,0.));
#27563=DIRECTION('',(0.,-1.,0.));
#27564=DIRECTION('center_axis',(-0.707106781186547,0.,0.707106781186548));
#27565=DIRECTION('ref_axis',(-0.707106781186548,0.,-0.707106781186547));
#27566=DIRECTION('',(0.,-1.,0.));
#27567=DIRECTION('',(0.707106781186548,0.,0.707106781186547));
#27568=DIRECTION('center_axis',(0.,-1.,0.));
#27569=DIRECTION('ref_axis',(1.,0.,0.));
#27570=DIRECTION('center_axis',(0.,1.,0.));
#27571=DIRECTION('ref_axis',(1.,0.,0.));
#27572=DIRECTION('center_axis',(0.,1.,0.));
#27573=DIRECTION('ref_axis',(0.,0.,1.));
#27574=DIRECTION('center_axis',(0.,0.,-1.));
#27575=DIRECTION('ref_axis',(0.,1.,0.));
#27576=DIRECTION('center_axis',(1.,0.,0.));
#27577=DIRECTION('ref_axis',(0.,0.,-1.));
#27578=DIRECTION('center_axis',(-1.,0.,0.));
#27579=DIRECTION('ref_axis',(0.,0.707106781186548,-0.707106781186548));
#27580=DIRECTION('center_axis',(1.,0.,-2.96059473233374E-15));
#27581=DIRECTION('ref_axis',(-2.96059473233374E-15,0.,-1.));
#27582=DIRECTION('center_axis',(0.,1.,0.));
#27583=DIRECTION('ref_axis',(0.,0.,1.));
#27584=DIRECTION('center_axis',(0.,0.,-1.));
#27585=DIRECTION('ref_axis',(-1.,0.,0.));
#27586=DIRECTION('center_axis',(0.,0.,1.));
#27587=DIRECTION('ref_axis',(-0.707106781186548,0.707106781186548,0.));
#27588=DIRECTION('center_axis',(-1.48029736616687E-15,0.,-1.));
#27589=DIRECTION('ref_axis',(-1.,0.,1.48029736616687E-15));
#27590=DIRECTION('center_axis',(0.,1.,0.));
#27591=DIRECTION('ref_axis',(0.,0.,1.));
#27592=DIRECTION('center_axis',(-1.,0.,0.));
#27593=DIRECTION('ref_axis',(0.,0.,1.));
#27594=DIRECTION('center_axis',(1.,0.,0.));
#27595=DIRECTION('ref_axis',(0.,0.707106781186548,0.707106781186548));
#27596=DIRECTION('center_axis',(-1.,0.,2.96059473233374E-15));
#27597=DIRECTION('ref_axis',(2.96059473233374E-15,0.,1.));
#27598=DIRECTION('',(1.,0.,0.));
#27599=DIRECTION('center_axis',(0.,1.,0.));
#27600=DIRECTION('ref_axis',(0.,0.,1.));
#27601=DIRECTION('center_axis',(0.,0.,1.));
#27602=DIRECTION('ref_axis',(1.,0.,0.));
#27603=DIRECTION('center_axis',(0.,1.,0.));
#27604=DIRECTION('ref_axis',(0.707106781186547,0.,0.707106781186548));
#27605=DIRECTION('center_axis',(0.,0.,-1.));
#27606=DIRECTION('ref_axis',(0.707106781186548,0.707106781186548,0.));
#27607=DIRECTION('',(0.,0.,-1.));
#27608=DIRECTION('center_axis',(0.,1.,0.));
#27609=DIRECTION('ref_axis',(1.22464679914735E-16,0.,1.));
#27610=DIRECTION('center_axis',(0.,-1.,0.));
#27611=DIRECTION('ref_axis',(1.22464679914735E-16,0.,1.));
#27612=DIRECTION('center_axis',(-1.,0.,-2.46519032881566E-32));
#27613=DIRECTION('ref_axis',(2.46519032881566E-32,0.,-1.));
#27614=DIRECTION('center_axis',(0.,1.,0.));
#27615=DIRECTION('ref_axis',(1.22464679914735E-16,0.,1.));
#27616=DIRECTION('center_axis',(0.,1.,0.));
#27617=DIRECTION('ref_axis',(0.,0.,1.));
#27618=DIRECTION('center_axis',(0.,1.,0.));
#27619=DIRECTION('ref_axis',(0.811029676142761,0.,0.585005012299696));
#27620=DIRECTION('center_axis',(0.,1.,0.));
#27621=DIRECTION('ref_axis',(-0.811029676142761,0.,0.585005012299696));
#27622=DIRECTION('',(0.,-1.,0.));
#27623=DIRECTION('center_axis',(0.,-1.,0.));
#27624=DIRECTION('ref_axis',(0.,0.,-1.));
#27625=DIRECTION('center_axis',(0.,1.,0.));
#27626=DIRECTION('ref_axis',(0.,0.,1.));
#27627=DIRECTION('center_axis',(5.04646829375071E-17,0.,-1.));
#27628=DIRECTION('ref_axis',(-0.707106781186548,-0.707106781186547,0.));
#27629=DIRECTION('',(5.04646829375071E-17,0.,-1.));
#27630=DIRECTION('center_axis',(-1.,0.,-5.04646829375071E-17));
#27631=DIRECTION('ref_axis',(5.04646829375071E-17,0.,-1.));
#27632=DIRECTION('',(-5.04646829375071E-17,0.,1.));
#27633=DIRECTION('center_axis',(0.,1.,0.));
#27634=DIRECTION('ref_axis',(0.,0.,1.));
#27635=DIRECTION('center_axis',(0.,-1.,0.));
#27636=DIRECTION('ref_axis',(0.,0.,-1.));
#27637=DIRECTION('center_axis',(0.,-1.,0.));
#27638=DIRECTION('ref_axis',(0.811029676142761,0.,0.585005012299696));
#27639=DIRECTION('center_axis',(0.,1.,0.));
#27640=DIRECTION('ref_axis',(1.,0.,0.));
#27641=DIRECTION('center_axis',(0.,1.,0.));
#27642=DIRECTION('ref_axis',(0.,0.,1.));
#27643=DIRECTION('center_axis',(0.,-1.,0.));
#27644=DIRECTION('ref_axis',(0.,0.,-1.));
#27645=DIRECTION('center_axis',(0.,-1.,0.));
#27646=DIRECTION('ref_axis',(-0.811029676142761,0.,0.585005012299696));
#27647=DIRECTION('center_axis',(0.,1.,0.));
#27648=DIRECTION('ref_axis',(1.,0.,0.));
#27649=DIRECTION('center_axis',(0.,0.,1.));
#27650=DIRECTION('ref_axis',(-0.707106781186545,0.70710678118655,0.));
#27651=DIRECTION('center_axis',(0.,0.,1.));
#27652=DIRECTION('ref_axis',(0.,1.,0.));
#27653=DIRECTION('',(0.,0.,1.));
#27654=DIRECTION('center_axis',(9.5625613772925E-16,0.,-1.));
#27655=DIRECTION('ref_axis',(-1.,0.,-9.5625613772925E-16));
#27656=DIRECTION('center_axis',(0.,-1.,0.));
#27657=DIRECTION('ref_axis',(-1.22464679914735E-16,0.,1.));
#27658=DIRECTION('center_axis',(0.,0.,1.));
#27659=DIRECTION('ref_axis',(1.,0.,0.));
#27660=DIRECTION('center_axis',(0.,-1.,0.));
#27661=DIRECTION('ref_axis',(-6.12323399573677E-17,0.,1.));
#27662=DIRECTION('center_axis',(0.,0.,-1.));
#27663=DIRECTION('ref_axis',(0.707106781186545,0.70710678118655,0.));
#27664=DIRECTION('center_axis',(0.,0.,1.));
#27665=DIRECTION('ref_axis',(1.,0.,0.));
#27666=DIRECTION('',(0.,0.,-1.));
#27667=DIRECTION('center_axis',(0.,-1.,0.));
#27668=DIRECTION('ref_axis',(0.,0.,-1.));
#27669=DIRECTION('center_axis',(0.,-1.,0.));
#27670=DIRECTION('ref_axis',(6.12323399573677E-17,0.,-1.));
#27671=DIRECTION('center_axis',(0.,-1.,0.));
#27672=DIRECTION('ref_axis',(-1.,0.,0.));
#27673=DIRECTION('',(0.,-1.,0.));
#27674=DIRECTION('center_axis',(0.,-1.,0.));
#27675=DIRECTION('ref_axis',(-1.,0.,0.));
#27676=DIRECTION('',(0.,-1.,0.));
#27677=DIRECTION('center_axis',(1.,0.,0.));
#27678=DIRECTION('ref_axis',(0.,0.,1.));
#27679=DIRECTION('',(0.,-1.,0.));
#27680=DIRECTION('',(0.,0.,1.));
#27681=DIRECTION('center_axis',(0.,0.,1.));
#27682=DIRECTION('ref_axis',(-0.707106781186545,0.70710678118655,0.));
#27683=DIRECTION('center_axis',(0.,0.,1.));
#27684=DIRECTION('ref_axis',(0.,1.,0.));
#27685=DIRECTION('',(0.,0.,1.));
#27686=DIRECTION('center_axis',(0.,0.,-1.));
#27687=DIRECTION('ref_axis',(-1.,0.,0.));
#27688=DIRECTION('center_axis',(0.,1.,0.));
#27689=DIRECTION('ref_axis',(0.,0.,1.));
#27690=DIRECTION('center_axis',(-1.22464679914735E-16,0.,1.));
#27691=DIRECTION('ref_axis',(1.,0.,1.22464679914735E-16));
#27692=DIRECTION('center_axis',(0.,1.,0.));
#27693=DIRECTION('ref_axis',(-6.12323399573676E-17,0.,1.));
#27694=DIRECTION('center_axis',(0.,0.,-1.));
#27695=DIRECTION('ref_axis',(0.707106781186545,0.70710678118655,0.));
#27696=DIRECTION('center_axis',(0.,0.,1.));
#27697=DIRECTION('ref_axis',(1.,0.,0.));
#27698=DIRECTION('',(0.,0.,-1.));
#27699=DIRECTION('center_axis',(0.,1.,0.));
#27700=DIRECTION('ref_axis',(-1.22464679914735E-16,0.,-1.));
#27701=DIRECTION('center_axis',(0.,1.,0.));
#27702=DIRECTION('ref_axis',(8.54643792476272E-17,0.,-1.));
#27703=DIRECTION('center_axis',(0.,-1.,0.));
#27704=DIRECTION('ref_axis',(-1.,0.,0.));
#27705=DIRECTION('',(0.,-1.,0.));
#27706=DIRECTION('center_axis',(0.,1.,0.));
#27707=DIRECTION('ref_axis',(-1.,0.,0.));
#27708=DIRECTION('',(0.,-1.,0.));
#27709=DIRECTION('center_axis',(1.,0.,0.));
#27710=DIRECTION('ref_axis',(0.,0.,1.));
#27711=DIRECTION('',(0.,-1.,0.));
#27712=DIRECTION('',(0.,0.,1.));
#27713=DIRECTION('center_axis',(0.,-1.,0.));
#27714=DIRECTION('ref_axis',(1.,0.,-1.97812565634772E-16));
#27715=DIRECTION('',(0.,-1.,0.));
#27716=DIRECTION('center_axis',(0.,1.,0.));
#27717=DIRECTION('ref_axis',(1.,0.,-1.97812565634772E-16));
#27718=DIRECTION('center_axis',(-1.,0.,0.));
#27719=DIRECTION('ref_axis',(0.,0.,-1.));
#27720=DIRECTION('',(0.,0.,-1.));
#27721=DIRECTION('center_axis',(0.,-1.,0.));
#27722=DIRECTION('ref_axis',(1.,0.,0.));
#27723=DIRECTION('',(0.,-1.,0.));
#27724=DIRECTION('center_axis',(0.,-1.,0.));
#27725=DIRECTION('ref_axis',(1.,0.,0.));
#27726=DIRECTION('center_axis',(-1.,0.,0.));
#27727=DIRECTION('ref_axis',(0.,0.,-1.));
#27728=DIRECTION('',(0.,0.,-1.));
#27729=DIRECTION('center_axis',(0.,1.,0.));
#27730=DIRECTION('ref_axis',(1.,0.,0.));
#27731=DIRECTION('center_axis',(0.,-1.,0.));
#27732=DIRECTION('ref_axis',(1.,0.,0.));
#27733=DIRECTION('',(0.,-1.,0.));
#27734=DIRECTION('center_axis',(0.,-1.,0.));
#27735=DIRECTION('ref_axis',(1.,0.,0.));
#27736=DIRECTION('center_axis',(0.,1.,0.));
#27737=DIRECTION('ref_axis',(1.,0.,0.));
#27738=DIRECTION('center_axis',(0.,-1.,0.));
#27739=DIRECTION('ref_axis',(1.,0.,0.));
#27740=DIRECTION('',(0.,-1.,0.));
#27741=DIRECTION('center_axis',(0.,-1.,0.));
#27742=DIRECTION('ref_axis',(1.,0.,0.));
#27743=DIRECTION('center_axis',(0.,1.,0.));
#27744=DIRECTION('ref_axis',(1.,0.,0.));
#27745=DIRECTION('center_axis',(0.,-1.,0.));
#27746=DIRECTION('ref_axis',(0.,0.,-1.));
#27747=DIRECTION('center_axis',(0.,1.,0.));
#27748=DIRECTION('ref_axis',(1.,0.,0.));
#27749=DIRECTION('center_axis',(0.,1.,0.));
#27750=DIRECTION('ref_axis',(0.,0.,1.));
#27751=DIRECTION('center_axis',(0.,1.,0.));
#27752=DIRECTION('ref_axis',(0.,0.,1.));
#27753=DIRECTION('',(0.,1.,0.));
#27754=DIRECTION('center_axis',(0.,1.,0.));
#27755=DIRECTION('ref_axis',(1.,0.,0.));
#27756=DIRECTION('center_axis',(0.,1.,0.));
#27757=DIRECTION('ref_axis',(0.,0.,1.));
#27758=DIRECTION('center_axis',(0.,-1.,0.));
#27759=DIRECTION('ref_axis',(0.,0.,1.));
#27760=DIRECTION('center_axis',(0.,1.,0.));
#27761=DIRECTION('ref_axis',(0.,0.,1.));
#27762=DIRECTION('',(0.,1.,0.));
#27763=DIRECTION('center_axis',(0.,1.,0.));
#27764=DIRECTION('ref_axis',(0.,0.,1.));
#27765=DIRECTION('',(0.,1.,0.));
#27766=DIRECTION('center_axis',(0.,1.,0.));
#27767=DIRECTION('ref_axis',(1.,0.,0.));
#27768=DIRECTION('center_axis',(0.,-1.,0.));
#27769=DIRECTION('ref_axis',(1.,0.,0.));
#27770=DIRECTION('center_axis',(0.,1.,0.));
#27771=DIRECTION('ref_axis',(1.,0.,0.));
#27772=DIRECTION('',(0.,1.,0.));
#27773=DIRECTION('center_axis',(0.,-1.,0.));
#27774=DIRECTION('ref_axis',(1.,0.,0.));
#27775=DIRECTION('center_axis',(0.,1.,0.));
#27776=DIRECTION('ref_axis',(1.,0.,0.));
#27777=DIRECTION('',(0.,1.,0.));
#27778=DIRECTION('center_axis',(0.,1.,0.));
#27779=DIRECTION('ref_axis',(1.,0.,0.));
#27780=DIRECTION('',(1.,0.,0.));
#27781=DIRECTION('center_axis',(0.,0.,1.));
#27782=DIRECTION('ref_axis',(1.,0.,0.));
#27783=DIRECTION('',(0.,1.,0.));
#27784=DIRECTION('center_axis',(-1.,0.,0.));
#27785=DIRECTION('ref_axis',(0.,0.,1.));
#27786=DIRECTION('',(0.,0.,1.));
#27787=DIRECTION('center_axis',(0.,0.,1.));
#27788=DIRECTION('ref_axis',(1.,0.,0.));
#27789=DIRECTION('',(1.,0.,0.));
#27790=DIRECTION('center_axis',(0.,1.,0.));
#27791=DIRECTION('ref_axis',(1.,0.,0.));
#27792=DIRECTION('center_axis',(0.,1.,0.));
#27793=DIRECTION('ref_axis',(1.,0.,0.));
#27794=DIRECTION('center_axis',(1.,0.,0.));
#27795=DIRECTION('ref_axis',(0.,0.,-1.));
#27796=DIRECTION('',(0.,1.,0.));
#27797=DIRECTION('center_axis',(0.,1.,0.));
#27798=DIRECTION('ref_axis',(4.75809867696496E-16,0.,1.));
#27799=DIRECTION('axis',(0.,0.,1.));
#27800=DIRECTION('refdir',(1.,0.,0.));
#27801=DIRECTION('center_axis',(1.,0.,0.));
#27802=DIRECTION('ref_axis',(0.,0.,-1.));
#27803=DIRECTION('center_axis',(1.,0.,0.));
#27804=DIRECTION('ref_axis',(0.,0.,-1.));
#27805=DIRECTION('',(-0.707106781186547,8.65956056235493E-17,-0.707106781186547));
#27806=DIRECTION('center_axis',(-1.,0.,0.));
#27807=DIRECTION('ref_axis',(0.,0.,-1.));
#27808=DIRECTION('center_axis',(-1.,0.,0.));
#27809=DIRECTION('ref_axis',(0.,0.,-1.));
#27810=DIRECTION('',(-1.,0.,0.));
#27811=DIRECTION('center_axis',(-1.,0.,0.));
#27812=DIRECTION('ref_axis',(0.,0.,-1.));
#27813=DIRECTION('center_axis',(1.,0.,0.));
#27814=DIRECTION('ref_axis',(0.,0.,-1.));
#27815=DIRECTION('center_axis',(-1.,0.,0.));
#27816=DIRECTION('ref_axis',(0.,0.,-1.));
#27817=DIRECTION('center_axis',(-1.,0.,0.));
#27818=DIRECTION('ref_axis',(0.,0.,-1.));
#27819=DIRECTION('center_axis',(-1.,0.,0.));
#27820=DIRECTION('ref_axis',(0.,0.,-1.));
#27821=DIRECTION('',(0.707106781186547,-8.65956056235493E-17,-0.707106781186547));
#27822=DIRECTION('center_axis',(1.,0.,0.));
#27823=DIRECTION('ref_axis',(0.,0.,-1.));
#27824=DIRECTION('center_axis',(1.,0.,0.));
#27825=DIRECTION('ref_axis',(0.,0.,-1.));
#27826=DIRECTION('',(1.,0.,0.));
#27827=DIRECTION('center_axis',(1.,0.,0.));
#27828=DIRECTION('ref_axis',(0.,0.,-1.));
#27829=DIRECTION('center_axis',(1.,0.,0.));
#27830=DIRECTION('ref_axis',(0.,0.,-1.));
#27831=DIRECTION('center_axis',(1.,0.,0.));
#27832=DIRECTION('ref_axis',(0.,0.,-1.));
#27833=DIRECTION('center_axis',(0.,0.,-1.));
#27834=DIRECTION('ref_axis',(0.707106781186555,0.70710678118654,0.));
#27835=DIRECTION('center_axis',(0.,0.,-1.));
#27836=DIRECTION('ref_axis',(0.,1.,0.));
#27837=DIRECTION('',(0.,0.,-1.));
#27838=DIRECTION('center_axis',(0.,0.,1.));
#27839=DIRECTION('ref_axis',(1.,0.,0.));
#27840=DIRECTION('',(0.,0.,1.));
#27841=DIRECTION('center_axis',(0.,1.,0.));
#27842=DIRECTION('ref_axis',(0.,0.,1.));
#27843=DIRECTION('center_axis',(1.,0.,0.));
#27844=DIRECTION('ref_axis',(0.,0.,-1.));
#27845=DIRECTION('center_axis',(0.,-1.,0.));
#27846=DIRECTION('ref_axis',(0.707106781186548,0.,-0.707106781186548));
#27847=DIRECTION('center_axis',(0.,1.,0.));
#27848=DIRECTION('ref_axis',(0.707106781186548,0.,-0.707106781186548));
#27849=DIRECTION('center_axis',(-1.,0.,0.));
#27850=DIRECTION('ref_axis',(0.,0.70710678118654,-0.707106781186555));
#27851=DIRECTION('center_axis',(1.,0.,-5.55111512312578E-15));
#27852=DIRECTION('ref_axis',(-5.55111512312578E-15,0.,-1.));
#27853=DIRECTION('',(1.,0.,0.));
#27854=DIRECTION('',(-1.,0.,0.));
#27855=DIRECTION('center_axis',(0.,1.,0.));
#27856=DIRECTION('ref_axis',(0.,0.,1.));
#27857=DIRECTION('center_axis',(0.,0.,-1.));
#27858=DIRECTION('ref_axis',(-1.,0.,0.));
#27859=DIRECTION('center_axis',(0.,-1.,0.));
#27860=DIRECTION('ref_axis',(-0.707106781186547,0.,-0.707106781186548));
#27861=DIRECTION('center_axis',(0.,1.,0.));
#27862=DIRECTION('ref_axis',(-0.707106781186547,0.,-0.707106781186548));
#27863=DIRECTION('center_axis',(0.,0.,1.));
#27864=DIRECTION('ref_axis',(-0.707106781186555,0.70710678118654,0.));
#27865=DIRECTION('center_axis',(0.,0.,-1.));
#27866=DIRECTION('ref_axis',(-1.,0.,0.));
#27867=DIRECTION('',(0.,0.,-1.));
#27868=DIRECTION('',(0.,0.,1.));
#27869=DIRECTION('center_axis',(0.,1.,0.));
#27870=DIRECTION('ref_axis',(0.,0.,1.));
#27871=DIRECTION('center_axis',(-1.,0.,0.));
#27872=DIRECTION('ref_axis',(0.,0.,1.));
#27873=DIRECTION('center_axis',(0.,-1.,0.));
#27874=DIRECTION('ref_axis',(-0.707106781186548,0.,0.707106781186548));
#27875=DIRECTION('center_axis',(0.,1.,0.));
#27876=DIRECTION('ref_axis',(-0.707106781186548,0.,0.707106781186548));
#27877=DIRECTION('center_axis',(1.,0.,0.));
#27878=DIRECTION('ref_axis',(0.,0.70710678118654,0.707106781186555));
#27879=DIRECTION('center_axis',(-1.,0.,5.55111512312578E-15));
#27880=DIRECTION('ref_axis',(5.55111512312578E-15,0.,1.));
#27881=DIRECTION('',(-1.,0.,0.));
#27882=DIRECTION('',(1.,0.,0.));
#27883=DIRECTION('center_axis',(0.,1.,0.));
#27884=DIRECTION('ref_axis',(0.,0.,1.));
#27885=DIRECTION('center_axis',(0.,-1.,0.));
#27886=DIRECTION('ref_axis',(0.707106781186548,0.,0.707106781186548));
#27887=DIRECTION('center_axis',(0.,1.,0.));
#27888=DIRECTION('ref_axis',(0.707106781186548,0.,0.707106781186548));
#27889=DIRECTION('center_axis',(0.,1.,0.));
#27890=DIRECTION('ref_axis',(1.33226762955019E-15,0.,-1.));
#27891=DIRECTION('',(0.,1.,0.));
#27892=DIRECTION('center_axis',(0.,-1.,0.));
#27893=DIRECTION('ref_axis',(-0.707106781186547,0.,-0.707106781186548));
#27894=DIRECTION('',(0.,1.,0.));
#27895=DIRECTION('center_axis',(0.,0.,-1.));
#27896=DIRECTION('ref_axis',(-1.,0.,0.));
#27897=DIRECTION('',(0.,1.,0.));
#27898=DIRECTION('',(1.,0.,0.));
#27899=DIRECTION('center_axis',(0.,1.,0.));
#27900=DIRECTION('ref_axis',(1.,0.,8.88178419700126E-16));
#27901=DIRECTION('',(0.,1.,0.));
#27902=DIRECTION('center_axis',(0.,-1.,0.));
#27903=DIRECTION('ref_axis',(0.707106781186548,0.,-0.707106781186548));
#27904=DIRECTION('center_axis',(1.,0.,0.));
#27905=DIRECTION('ref_axis',(0.,0.,-1.));
#27906=DIRECTION('',(0.,1.,0.));
#27907=DIRECTION('',(0.,0.,1.));
#27908=DIRECTION('center_axis',(-1.,0.,0.));
#27909=DIRECTION('ref_axis',(0.,0.,-1.));
#27910=DIRECTION('center_axis',(0.,1.,0.));
#27911=DIRECTION('ref_axis',(1.,0.,0.));
#27912=DIRECTION('center_axis',(0.,-1.,0.));
#27913=DIRECTION('ref_axis',(1.,0.,0.));
#27914=DIRECTION('center_axis',(0.,-1.,0.));
#27915=DIRECTION('ref_axis',(1.,0.,0.));
#27916=DIRECTION('center_axis',(0.,-1.,0.));
#27917=DIRECTION('ref_axis',(1.,0.,0.));
#27918=DIRECTION('center_axis',(0.,-1.,0.));
#27919=DIRECTION('ref_axis',(1.,0.,0.));
#27920=DIRECTION('center_axis',(0.,-1.,0.));
#27921=DIRECTION('ref_axis',(1.,0.,0.));
#27922=DIRECTION('center_axis',(0.,-1.,0.));
#27923=DIRECTION('ref_axis',(1.,0.,0.));
#27924=DIRECTION('center_axis',(0.,-1.,0.));
#27925=DIRECTION('ref_axis',(1.,0.,0.));
#27926=DIRECTION('center_axis',(0.,-1.,0.));
#27927=DIRECTION('ref_axis',(1.,0.,0.));
#27928=DIRECTION('center_axis',(0.,0.,1.));
#27929=DIRECTION('ref_axis',(0.707106781186548,-0.707106781186548,0.));
#27930=DIRECTION('center_axis',(0.,0.,1.));
#27931=DIRECTION('ref_axis',(0.,-1.,0.));
#27932=DIRECTION('center_axis',(0.,0.,-1.));
#27933=DIRECTION('ref_axis',(1.,0.,0.));
#27934=DIRECTION('',(0.,0.,-1.));
#27935=DIRECTION('center_axis',(0.,1.,0.));
#27936=DIRECTION('ref_axis',(0.,0.,1.));
#27937=DIRECTION('center_axis',(1.,0.,0.));
#27938=DIRECTION('ref_axis',(0.,0.,1.));
#27939=DIRECTION('center_axis',(0.,1.,0.));
#27940=DIRECTION('ref_axis',(0.707106781186548,0.,0.707106781186548));
#27941=DIRECTION('center_axis',(0.,-1.,0.));
#27942=DIRECTION('ref_axis',(0.707106781186548,0.,0.707106781186548));
#27943=DIRECTION('center_axis',(-1.,0.,0.));
#27944=DIRECTION('ref_axis',(0.,-0.707106781186548,0.707106781186548));
#27945=DIRECTION('center_axis',(1.,0.,0.));
#27946=DIRECTION('ref_axis',(0.,0.,1.));
#27947=DIRECTION('',(1.,0.,0.));
#27948=DIRECTION('',(-1.,0.,0.));
#27949=DIRECTION('center_axis',(0.,1.,0.));
#27950=DIRECTION('ref_axis',(0.,0.,1.));
#27951=DIRECTION('center_axis',(5.55111512312581E-15,0.,1.));
#27952=DIRECTION('ref_axis',(-1.,0.,5.55111512312581E-15));
#27953=DIRECTION('center_axis',(0.,1.,0.));
#27954=DIRECTION('ref_axis',(-0.707106781186548,0.,0.707106781186548));
#27955=DIRECTION('center_axis',(0.,-1.,0.));
#27956=DIRECTION('ref_axis',(-0.707106781186548,0.,0.707106781186548));
#27957=DIRECTION('center_axis',(0.,0.,-1.));
#27958=DIRECTION('ref_axis',(-0.707106781186548,-0.707106781186548,0.));
#27959=DIRECTION('center_axis',(0.,0.,1.));
#27960=DIRECTION('ref_axis',(-1.,0.,0.));
#27961=DIRECTION('',(0.,0.,1.));
#27962=DIRECTION('',(0.,0.,-1.));
#27963=DIRECTION('center_axis',(0.,1.,0.));
#27964=DIRECTION('ref_axis',(0.,0.,1.));
#27965=DIRECTION('center_axis',(-1.,0.,-5.55111512312578E-15));
#27966=DIRECTION('ref_axis',(5.55111512312578E-15,0.,-1.));
#27967=DIRECTION('center_axis',(0.,1.,0.));
#27968=DIRECTION('ref_axis',(-0.707106781186547,0.,-0.707106781186548));
#27969=DIRECTION('center_axis',(1.,0.,0.));
#27970=DIRECTION('ref_axis',(0.,-0.707106781186548,-0.707106781186548));
#27971=DIRECTION('center_axis',(-1.,0.,0.));
#27972=DIRECTION('ref_axis',(0.,0.,-1.));
#27973=DIRECTION('',(-1.,0.,0.));
#27974=DIRECTION('center_axis',(0.,1.,0.));
#27975=DIRECTION('ref_axis',(0.,0.,1.));
#27976=DIRECTION('center_axis',(0.,1.,0.));
#27977=DIRECTION('ref_axis',(0.707106781186548,0.,-0.707106781186548));
#27978=DIRECTION('center_axis',(0.,1.,0.));
#27979=DIRECTION('ref_axis',(-1.,0.,-8.88178419700126E-16));
#27980=DIRECTION('',(0.,1.,0.));
#27981=DIRECTION('',(0.,1.,0.));
#27982=DIRECTION('center_axis',(0.,0.,1.));
#27983=DIRECTION('ref_axis',(1.,0.,0.));
#27984=DIRECTION('',(0.,1.,0.));
#27985=DIRECTION('center_axis',(0.,1.,0.));
#27986=DIRECTION('ref_axis',(-4.44089209850063E-16,0.,1.));
#27987=DIRECTION('center_axis',(0.,1.,0.));
#27988=DIRECTION('ref_axis',(1.,0.,0.));
#27989=DIRECTION('center_axis',(0.,1.,0.));
#27990=DIRECTION('ref_axis',(1.,0.,0.));
#27991=DIRECTION('center_axis',(0.,1.,0.));
#27992=DIRECTION('ref_axis',(1.,0.,0.));
#27993=DIRECTION('center_axis',(0.,1.,0.));
#27994=DIRECTION('ref_axis',(1.,0.,0.));
#27995=DIRECTION('center_axis',(0.,1.,0.));
#27996=DIRECTION('ref_axis',(1.,0.,0.));
#27997=DIRECTION('center_axis',(0.,1.,0.));
#27998=DIRECTION('ref_axis',(1.,0.,0.));
#27999=DIRECTION('center_axis',(0.,1.,0.));
#28000=DIRECTION('ref_axis',(1.,0.,0.));
#28001=DIRECTION('center_axis',(0.,1.,0.));
#28002=DIRECTION('ref_axis',(1.,0.,0.));
#28003=DIRECTION('center_axis',(0.,1.,0.));
#28004=DIRECTION('ref_axis',(1.,0.,0.));
#28005=DIRECTION('center_axis',(0.,-1.,0.));
#28006=DIRECTION('ref_axis',(1.,0.,0.));
#28007=DIRECTION('',(0.,-1.,0.));
#28008=DIRECTION('center_axis',(0.,-1.,0.));
#28009=DIRECTION('ref_axis',(1.,0.,0.));
#28010=DIRECTION('center_axis',(0.,1.,0.));
#28011=DIRECTION('ref_axis',(1.,0.,0.));
#28012=DIRECTION('center_axis',(0.,-1.,0.));
#28013=DIRECTION('ref_axis',(1.,0.,0.));
#28014=DIRECTION('',(0.,-1.,0.));
#28015=DIRECTION('center_axis',(0.,-1.,0.));
#28016=DIRECTION('ref_axis',(1.,0.,0.));
#28017=DIRECTION('center_axis',(0.,1.,0.));
#28018=DIRECTION('ref_axis',(1.,0.,0.));
#28019=DIRECTION('center_axis',(0.,1.,0.));
#28020=DIRECTION('ref_axis',(1.,0.,0.));
#28021=DIRECTION('',(0.,1.,0.));
#28022=DIRECTION('center_axis',(0.,1.,0.));
#28023=DIRECTION('ref_axis',(1.,0.,0.));
#28024=DIRECTION('center_axis',(0.,1.,0.));
#28025=DIRECTION('ref_axis',(1.,0.,0.));
#28026=DIRECTION('center_axis',(0.,1.,0.));
#28027=DIRECTION('ref_axis',(1.,0.,0.));
#28028=DIRECTION('',(0.,1.,0.));
#28029=DIRECTION('center_axis',(0.,1.,0.));
#28030=DIRECTION('ref_axis',(1.,0.,0.));
#28031=DIRECTION('center_axis',(0.,1.,0.));
#28032=DIRECTION('ref_axis',(1.,0.,0.));
#28033=DIRECTION('center_axis',(0.,1.,0.));
#28034=DIRECTION('ref_axis',(1.,0.,0.));
#28035=DIRECTION('',(0.,1.,0.));
#28036=DIRECTION('center_axis',(0.,1.,0.));
#28037=DIRECTION('ref_axis',(1.,0.,0.));
#28038=DIRECTION('',(0.,1.,0.));
#28039=DIRECTION('center_axis',(0.,1.,0.));
#28040=DIRECTION('ref_axis',(1.,0.,0.));
#28041=DIRECTION('',(0.,1.,0.));
#28042=DIRECTION('center_axis',(0.,1.,0.));
#28043=DIRECTION('ref_axis',(1.,0.,0.));
#28044=DIRECTION('',(0.,1.,0.));
#28045=DIRECTION('center_axis',(1.,0.,0.));
#28046=DIRECTION('ref_axis',(0.,0.,-1.));
#28047=DIRECTION('center_axis',(1.,0.,0.));
#28048=DIRECTION('ref_axis',(0.,0.,-1.));
#28049=DIRECTION('',(1.,0.,0.));
#28050=DIRECTION('center_axis',(0.,1.,0.));
#28051=DIRECTION('ref_axis',(-1.83697019872103E-16,0.,1.));
#28052=DIRECTION('',(0.,1.,0.));
#28053=DIRECTION('',(0.,1.,0.));
#28054=DIRECTION('',(0.,1.,0.));
#28055=DIRECTION('',(0.,1.,0.));
#28056=DIRECTION('center_axis',(1.,0.,0.));
#28057=DIRECTION('ref_axis',(0.,0.,-1.));
#28058=DIRECTION('center_axis',(1.,0.,0.));
#28059=DIRECTION('ref_axis',(0.,0.,-1.));
#28060=DIRECTION('center_axis',(1.,0.,0.));
#28061=DIRECTION('ref_axis',(0.,0.,-1.));
#28062=DIRECTION('',(1.,0.,0.));
#28063=DIRECTION('center_axis',(-1.,0.,0.));
#28064=DIRECTION('ref_axis',(0.,0.,-1.));
#28065=DIRECTION('center_axis',(-1.,0.,0.));
#28066=DIRECTION('ref_axis',(0.,0.,-1.));
#28067=DIRECTION('',(-1.,0.,0.));
#28068=DIRECTION('center_axis',(0.,1.,0.));
#28069=DIRECTION('ref_axis',(-1.83697019872103E-16,0.,-1.));
#28070=DIRECTION('center_axis',(1.,0.,0.));
#28071=DIRECTION('ref_axis',(0.,0.,-1.));
#28072=DIRECTION('center_axis',(-1.,0.,0.));
#28073=DIRECTION('ref_axis',(0.,0.,-1.));
#28074=DIRECTION('',(-1.,0.,0.));
#28075=DIRECTION('center_axis',(-1.,0.,0.));
#28076=DIRECTION('ref_axis',(0.,0.,1.));
#28077=DIRECTION('axis',(0.,0.,1.));
#28078=DIRECTION('refdir',(1.,0.,0.));
#28079=DIRECTION('center_axis',(0.,1.,0.));
#28080=DIRECTION('ref_axis',(1.,0.,0.));
#28081=DIRECTION('center_axis',(0.,-1.,0.));
#28082=DIRECTION('ref_axis',(1.,0.,0.));
#28083=DIRECTION('',(-0.707106781186543,0.707106781186552,-8.65956056235488E-17));
#28084=DIRECTION('center_axis',(0.,1.,0.));
#28085=DIRECTION('ref_axis',(1.,0.,0.));
#28086=DIRECTION('center_axis',(0.,1.,0.));
#28087=DIRECTION('ref_axis',(1.,0.,0.));
#28088=DIRECTION('center_axis',(0.,-1.,0.));
#28089=DIRECTION('ref_axis',(1.,0.,0.));
#28090=DIRECTION('center_axis',(0.,-1.,0.));
#28091=DIRECTION('ref_axis',(1.,0.,0.));
#28092=DIRECTION('',(0.,-1.,0.));
#28093=DIRECTION('center_axis',(0.,-1.,0.));
#28094=DIRECTION('ref_axis',(1.,0.,0.));
#28095=DIRECTION('center_axis',(0.707106781186554,-0.707106781186541,0.));
#28096=DIRECTION('ref_axis',(0.,0.,-1.));
#28097=DIRECTION('',(-0.707106781186541,-0.707106781186554,0.));
#28098=DIRECTION('',(0.,0.,-1.));
#28099=DIRECTION('',(0.707106781186541,0.707106781186554,0.));
#28100=DIRECTION('',(0.,0.,1.));
#28101=DIRECTION('center_axis',(0.,-1.,0.));
#28102=DIRECTION('ref_axis',(-1.,0.,0.));
#28103=DIRECTION('',(0.707106781186541,-0.707106781186554,8.65956056235483E-17));
#28104=DIRECTION('center_axis',(0.,-1.,0.));
#28105=DIRECTION('ref_axis',(-1.,0.,0.));
#28106=DIRECTION('center_axis',(0.,1.,0.));
#28107=DIRECTION('ref_axis',(-1.,0.,0.));
#28108=DIRECTION('center_axis',(-0.707106781186554,-0.707106781186541,0.));
#28109=DIRECTION('ref_axis',(0.,0.,1.));
#28110=DIRECTION('',(0.707106781186541,-0.707106781186554,0.));
#28111=DIRECTION('',(0.,0.,1.));
#28112=DIRECTION('',(0.,0.,-1.));
#28113=DIRECTION('center_axis',(0.,-1.,0.));
#28114=DIRECTION('ref_axis',(1.,0.,0.));
#28115=DIRECTION('center_axis',(0.,-1.,0.));
#28116=DIRECTION('ref_axis',(1.,0.,0.));
#28117=DIRECTION('center_axis',(0.,1.,0.));
#28118=DIRECTION('ref_axis',(1.,0.,0.));
#28119=DIRECTION('center_axis',(0.,1.,0.));
#28120=DIRECTION('ref_axis',(-1.,0.,0.));
#28121=DIRECTION('',(0.,1.,0.));
#28122=DIRECTION('center_axis',(0.,1.,0.));
#28123=DIRECTION('ref_axis',(-1.,0.,0.));
#28124=DIRECTION('',(0.,1.,0.));
#28125=DIRECTION('center_axis',(-1.,0.,0.));
#28126=DIRECTION('ref_axis',(0.,0.,1.));
#28127=DIRECTION('',(0.,1.,0.));
#28128=DIRECTION('',(0.,0.,1.));
#28129=DIRECTION('center_axis',(0.,1.,0.));
#28130=DIRECTION('ref_axis',(1.,0.,0.));
#28131=DIRECTION('center_axis',(0.,1.,0.));
#28132=DIRECTION('ref_axis',(1.33226762955019E-15,0.,-1.));
#28133=DIRECTION('',(-1.,0.,0.));
#28134=DIRECTION('center_axis',(0.,1.,0.));
#28135=DIRECTION('ref_axis',(1.,0.,8.88178419700126E-16));
#28136=DIRECTION('',(0.,0.,-1.));
#28137=DIRECTION('center_axis',(0.,1.,0.));
#28138=DIRECTION('ref_axis',(-4.44089209850063E-16,0.,1.));
#28139=DIRECTION('',(1.,0.,0.));
#28140=DIRECTION('center_axis',(0.,1.,0.));
#28141=DIRECTION('ref_axis',(-1.,0.,-8.88178419700126E-16));
#28142=DIRECTION('',(0.,0.,1.));
#28143=DIRECTION('center_axis',(0.,1.,0.));
#28144=DIRECTION('ref_axis',(1.,0.,0.));
#28145=DIRECTION('center_axis',(0.,1.,0.));
#28146=DIRECTION('ref_axis',(1.,0.,0.));
#28147=DIRECTION('center_axis',(0.,1.,0.));
#28148=DIRECTION('ref_axis',(1.,0.,0.));
#28149=DIRECTION('center_axis',(0.,1.,0.));
#28150=DIRECTION('ref_axis',(1.,0.,0.));
#28151=DIRECTION('center_axis',(0.,1.,0.));
#28152=DIRECTION('ref_axis',(1.,0.,0.));
#28153=DIRECTION('center_axis',(0.,1.,0.));
#28154=DIRECTION('ref_axis',(1.,0.,0.));
#28155=DIRECTION('center_axis',(0.707106781186554,-0.707106781186541,0.));
#28156=DIRECTION('ref_axis',(0.,0.,-1.));
#28157=DIRECTION('',(-0.707106781186541,-0.707106781186554,2.39222714223772E-15));
#28158=DIRECTION('',(0.,0.,-1.));
#28159=DIRECTION('',(0.707106781186541,0.707106781186554,0.));
#28160=DIRECTION('',(0.,0.,1.));
#28161=DIRECTION('center_axis',(0.,1.,0.));
#28162=DIRECTION('ref_axis',(-1.,0.,0.));
#28163=DIRECTION('',(0.707106781186541,-0.707106781186554,7.60309417374759E-15));
#28164=DIRECTION('center_axis',(0.,1.,0.));
#28165=DIRECTION('ref_axis',(-1.,0.,0.));
#28166=DIRECTION('center_axis',(0.,-1.,0.));
#28167=DIRECTION('ref_axis',(-1.,0.,0.));
#28168=DIRECTION('center_axis',(-0.707106781186554,-0.707106781186541,0.));
#28169=DIRECTION('ref_axis',(0.,0.,1.));
#28170=DIRECTION('',(0.707106781186541,-0.707106781186554,0.));
#28171=DIRECTION('',(0.,0.,1.));
#28172=DIRECTION('',(0.,0.,-1.));
#28173=DIRECTION('center_axis',(0.,1.,0.));
#28174=DIRECTION('ref_axis',(1.,0.,-1.97812565634772E-16));
#28175=DIRECTION('center_axis',(0.,1.,0.));
#28176=DIRECTION('ref_axis',(1.,0.,-1.97812565634772E-16));
#28177=DIRECTION('center_axis',(0.,-1.,0.));
#28178=DIRECTION('ref_axis',(1.,0.,-1.97812565634772E-16));
#28179=DIRECTION('center_axis',(0.,1.,0.));
#28180=DIRECTION('ref_axis',(-1.,0.,0.));
#28181=DIRECTION('',(0.,1.,0.));
#28182=DIRECTION('center_axis',(0.,-1.,0.));
#28183=DIRECTION('ref_axis',(-1.,0.,0.));
#28184=DIRECTION('',(0.,1.,0.));
#28185=DIRECTION('center_axis',(-1.,0.,0.));
#28186=DIRECTION('ref_axis',(0.,0.,1.));
#28187=DIRECTION('',(0.,1.,0.));
#28188=DIRECTION('',(0.,0.,1.));
#28189=DIRECTION('center_axis',(0.,1.,0.));
#28190=DIRECTION('ref_axis',(1.,0.,0.));
#28191=DIRECTION('center_axis',(0.,1.,0.));
#28192=DIRECTION('ref_axis',(1.,0.,0.));
#28193=DIRECTION('',(0.707106781186541,-0.707106781186554,-8.65956056235486E-17));
#28194=DIRECTION('center_axis',(0.,-1.,0.));
#28195=DIRECTION('ref_axis',(1.,0.,0.));
#28196=DIRECTION('center_axis',(0.,1.,0.));
#28197=DIRECTION('ref_axis',(1.,0.,0.));
#28198=DIRECTION('center_axis',(-0.707106781186549,0.707106781186546,0.));
#28199=DIRECTION('ref_axis',(0.,0.,1.));
#28200=DIRECTION('',(0.,0.,-1.));
#28201=DIRECTION('',(0.,0.,-1.));
#28202=DIRECTION('',(0.707106781186548,0.707106781186548,0.));
#28203=DIRECTION('',(0.,0.,-1.));
#28204=DIRECTION('',(0.707106781186546,0.707106781186549,0.));
#28205=DIRECTION('',(0.,0.,-1.));
#28206=DIRECTION('center_axis',(0.,-1.,0.));
#28207=DIRECTION('ref_axis',(1.,0.,0.));
#28208=DIRECTION('',(0.,-1.,0.));
#28209=DIRECTION('center_axis',(0.,-1.,0.));
#28210=DIRECTION('ref_axis',(1.,0.,0.));
#28211=DIRECTION('center_axis',(0.,1.,0.));
#28212=DIRECTION('ref_axis',(1.,0.,0.));
#28213=DIRECTION('',(0.707106781186541,-0.707106781186554,-8.65956056235486E-17));
#28214=DIRECTION('center_axis',(0.,-1.,0.));
#28215=DIRECTION('ref_axis',(1.,0.,0.));
#28216=DIRECTION('center_axis',(0.,1.,0.));
#28217=DIRECTION('ref_axis',(1.,0.,0.));
#28218=DIRECTION('center_axis',(0.,-1.,0.));
#28219=DIRECTION('ref_axis',(1.,0.,0.));
#28220=DIRECTION('',(0.,-1.,0.));
#28221=DIRECTION('center_axis',(0.,-1.,0.));
#28222=DIRECTION('ref_axis',(1.,0.,0.));
#28223=DIRECTION('center_axis',(0.,1.,0.));
#28224=DIRECTION('ref_axis',(-1.,0.,0.));
#28225=DIRECTION('',(-0.707106781186541,-0.707106781186554,8.65956056235486E-17));
#28226=DIRECTION('center_axis',(0.,-1.,0.));
#28227=DIRECTION('ref_axis',(-1.,0.,0.));
#28228=DIRECTION('center_axis',(0.,-1.,0.));
#28229=DIRECTION('ref_axis',(-1.,0.,0.));
#28230=DIRECTION('center_axis',(0.,1.,0.));
#28231=DIRECTION('ref_axis',(-1.,0.,0.));
#28232=DIRECTION('center_axis',(0.707106781186549,0.707106781186546,0.));
#28233=DIRECTION('ref_axis',(0.,0.,-1.));
#28234=DIRECTION('',(0.,0.,1.));
#28235=DIRECTION('',(0.,0.,1.));
#28236=DIRECTION('',(0.707106781186544,-0.707106781186551,0.));
#28237=DIRECTION('',(0.,0.,1.));
#28238=DIRECTION('',(-0.707106781186546,0.707106781186549,0.));
#28239=DIRECTION('',(0.,0.,1.));
#28240=DIRECTION('center_axis',(0.,-1.,0.));
#28241=DIRECTION('ref_axis',(1.,0.,0.));
#28242=DIRECTION('',(0.,-1.,0.));
#28243=DIRECTION('center_axis',(0.,-1.,0.));
#28244=DIRECTION('ref_axis',(1.,0.,0.));
#28245=DIRECTION('center_axis',(0.,1.,0.));
#28246=DIRECTION('ref_axis',(-1.,0.,0.));
#28247=DIRECTION('',(-0.707106781186541,-0.707106781186554,8.65956056235486E-17));
#28248=DIRECTION('center_axis',(0.,-1.,0.));
#28249=DIRECTION('ref_axis',(-1.,0.,0.));
#28250=DIRECTION('center_axis',(0.,-1.,0.));
#28251=DIRECTION('ref_axis',(-1.,0.,0.));
#28252=DIRECTION('center_axis',(0.,1.,0.));
#28253=DIRECTION('ref_axis',(-1.,0.,0.));
#28254=DIRECTION('center_axis',(0.,-1.,0.));
#28255=DIRECTION('ref_axis',(1.,0.,0.));
#28256=DIRECTION('',(0.,-1.,0.));
#28257=DIRECTION('center_axis',(0.,-1.,0.));
#28258=DIRECTION('ref_axis',(1.,0.,0.));
#28259=DIRECTION('center_axis',(0.,1.,0.));
#28260=DIRECTION('ref_axis',(1.33226762955019E-15,0.,-1.));
#28261=DIRECTION('',(-0.707106781186547,0.707106781186547,0.));
#28262=DIRECTION('center_axis',(0.,-1.,0.));
#28263=DIRECTION('ref_axis',(1.33226762955019E-15,0.,-1.));
#28264=DIRECTION('',(0.,-0.707106781186554,0.707106781186541));
#28265=DIRECTION('center_axis',(-0.707106781186554,-0.707106781186541,0.));
#28266=DIRECTION('ref_axis',(0.,0.,1.));
#28267=DIRECTION('',(-0.707106781186541,0.707106781186554,0.));
#28268=DIRECTION('',(0.,0.,-1.));
#28269=DIRECTION('center_axis',(0.,1.,0.));
#28270=DIRECTION('ref_axis',(-1.,0.,-8.88178419700126E-16));
#28271=DIRECTION('',(0.,0.707106781186554,0.707106781186541));
#28272=DIRECTION('center_axis',(0.,-1.,0.));
#28273=DIRECTION('ref_axis',(-1.,0.,-8.88178419700126E-16));
#28274=DIRECTION('center_axis',(0.,-0.707106781186541,0.707106781186554));
#28275=DIRECTION('ref_axis',(1.,0.,0.));
#28276=DIRECTION('',(6.28036983473507E-15,0.707106781186554,0.707106781186541));
#28277=DIRECTION('',(-1.,0.,0.));
#28278=DIRECTION('center_axis',(0.,1.,0.));
#28279=DIRECTION('ref_axis',(-4.44089209850063E-16,0.,1.));
#28280=DIRECTION('',(0.707106781186538,0.707106781186557,0.));
#28281=DIRECTION('center_axis',(0.,-1.,0.));
#28282=DIRECTION('ref_axis',(-4.44089209850063E-16,0.,1.));
#28283=DIRECTION('center_axis',(0.707106781186554,-0.707106781186541,0.));
#28284=DIRECTION('ref_axis',(0.,0.,-1.));
#28285=DIRECTION('',(0.707106781186541,0.707106781186554,0.));
#28286=DIRECTION('',(0.,0.,1.));
#28287=DIRECTION('center_axis',(0.,1.,0.));
#28288=DIRECTION('ref_axis',(1.,0.,8.88178419700126E-16));
#28289=DIRECTION('',(0.,0.707106781186554,-0.707106781186541));
#28290=DIRECTION('center_axis',(0.,-1.,0.));
#28291=DIRECTION('ref_axis',(1.,0.,8.88178419700126E-16));
#28292=DIRECTION('center_axis',(0.,-0.707106781186541,-0.707106781186554));
#28293=DIRECTION('ref_axis',(-1.,0.,0.));
#28294=DIRECTION('',(1.,0.,0.));
#28295=DIRECTION('center_axis',(1.,0.,0.));
#28296=DIRECTION('ref_axis',(0.,0.,-1.));
#28297=DIRECTION('',(0.,1.,0.));
#28298=DIRECTION('',(0.,0.,-1.));
#28299=DIRECTION('',(0.,1.,0.));
#28300=DIRECTION('center_axis',(0.,1.,0.));
#28301=DIRECTION('ref_axis',(1.,0.,8.88178419700126E-16));
#28302=DIRECTION('',(0.,1.,0.));
#28303=DIRECTION('center_axis',(0.,1.,0.));
#28304=DIRECTION('ref_axis',(1.,0.,8.88178419700126E-16));
#28305=DIRECTION('center_axis',(0.,0.,-1.));
#28306=DIRECTION('ref_axis',(-1.,0.,0.));
#28307=DIRECTION('',(0.,1.,0.));
#28308=DIRECTION('',(-1.,0.,0.));
#28309=DIRECTION('center_axis',(0.,1.,0.));
#28310=DIRECTION('ref_axis',(1.33226762955019E-15,0.,-1.));
#28311=DIRECTION('',(0.,1.,0.));
#28312=DIRECTION('center_axis',(0.,1.,0.));
#28313=DIRECTION('ref_axis',(1.33226762955019E-15,0.,-1.));
#28314=DIRECTION('center_axis',(0.923879532511288,0.382683432365087,0.));
#28315=DIRECTION('ref_axis',(0.,0.,-1.));
#28316=DIRECTION('',(-0.382683432365087,0.923879532511288,0.));
#28317=DIRECTION('',(0.382683432365078,-0.923879532511291,0.));
#28318=DIRECTION('center_axis',(5.20282872453227E-15,-1.,0.));
#28319=DIRECTION('ref_axis',(1.,0.,9.04161894879113E-16));
#28320=DIRECTION('',(0.,0.923879532511288,0.382683432365087));
#28321=DIRECTION('center_axis',(0.,-1.,0.));
#28322=DIRECTION('ref_axis',(1.,0.,9.20731182852366E-16));
#28323=DIRECTION('center_axis',(0.,0.382683432365087,-0.923879532511288));
#28324=DIRECTION('ref_axis',(-1.,0.,0.));
#28325=DIRECTION('',(0.,0.923879532511282,0.382683432365102));
#28326=DIRECTION('',(1.,0.,0.));
#28327=DIRECTION('center_axis',(0.,-1.,0.));
#28328=DIRECTION('ref_axis',(1.35624284231867E-15,0.,-1.));
#28329=DIRECTION('',(0.382683432365103,0.923879532511281,0.));
#28330=DIRECTION('center_axis',(0.,-1.,0.));
#28331=DIRECTION('ref_axis',(1.38109677427855E-15,0.,-1.));
#28332=DIRECTION('center_axis',(-0.923879532511288,0.382683432365087,0.));
#28333=DIRECTION('ref_axis',(0.,0.,1.));
#28334=DIRECTION('',(0.382683432365087,0.923879532511288,0.));
#28335=DIRECTION('',(0.,0.,1.));
#28336=DIRECTION('center_axis',(0.,-1.,0.));
#28337=DIRECTION('ref_axis',(-1.,0.,-9.04161894879113E-16));
#28338=DIRECTION('',(0.,0.923879532511288,-0.382683432365087));
#28339=DIRECTION('center_axis',(0.,-1.,0.));
#28340=DIRECTION('ref_axis',(-1.,0.,-9.20731182852366E-16));
#28341=DIRECTION('center_axis',(0.,1.,0.));
#28342=DIRECTION('ref_axis',(-1.,0.,-8.88178419700126E-16));
#28343=DIRECTION('center_axis',(0.,0.382683432365083,0.92387953251129));
#28344=DIRECTION('ref_axis',(1.,0.,0.));
#28345=DIRECTION('',(0.,0.92387953251129,-0.382683432365083));
#28346=DIRECTION('',(-1.,0.,0.));
#28347=DIRECTION('',(1.,0.,0.));
#28348=DIRECTION('center_axis',(0.,-1.,0.));
#28349=DIRECTION('ref_axis',(-4.52080947439557E-16,0.,1.));
#28350=DIRECTION('center_axis',(0.,-1.,0.));
#28351=DIRECTION('ref_axis',(-4.60365591426184E-16,0.,1.));
#28352=DIRECTION('center_axis',(0.,1.,0.));
#28353=DIRECTION('ref_axis',(-4.44089209850063E-16,0.,1.));
#28354=DIRECTION('center_axis',(0.,-1.,0.));
#28355=DIRECTION('ref_axis',(-1.,0.,-8.88178419700126E-16));
#28356=DIRECTION('',(-2.09345661157836E-15,0.707106781186549,-0.707106781186546));
#28357=DIRECTION('center_axis',(0.,-1.,0.));
#28358=DIRECTION('ref_axis',(-1.,0.,-8.88178419700126E-16));
#28359=DIRECTION('center_axis',(0.,0.707106781186546,0.707106781186549));
#28360=DIRECTION('ref_axis',(1.,0.,0.));
#28361=DIRECTION('',(-2.09345661157836E-15,0.707106781186549,-0.707106781186546));
#28362=DIRECTION('',(-1.,0.,0.));
#28363=DIRECTION('center_axis',(0.,-1.,0.));
#28364=DIRECTION('ref_axis',(-4.44089209850063E-16,0.,1.));
#28365=DIRECTION('center_axis',(0.,-1.,0.));
#28366=DIRECTION('ref_axis',(-4.44089209850063E-16,0.,1.));
#28367=DIRECTION('center_axis',(0.,-1.,0.));
#28368=DIRECTION('ref_axis',(1.,0.,8.88178419700126E-16));
#28369=DIRECTION('',(2.09345661157837E-15,0.70710678118655,0.707106781186545));
#28370=DIRECTION('center_axis',(0.,-1.,0.));
#28371=DIRECTION('ref_axis',(1.,0.,8.88178419700126E-16));
#28372=DIRECTION('center_axis',(0.,0.707106781186548,-0.707106781186548));
#28373=DIRECTION('ref_axis',(-1.,0.,0.));
#28374=DIRECTION('',(2.09345661157836E-15,0.707106781186548,0.707106781186548));
#28375=DIRECTION('',(1.,0.,0.));
#28376=DIRECTION('center_axis',(0.,-1.,0.));
#28377=DIRECTION('ref_axis',(1.33226762955019E-15,0.,-1.));
#28378=DIRECTION('center_axis',(0.,-1.,0.));
#28379=DIRECTION('ref_axis',(1.33226762955019E-15,0.,-1.));
#28380=DIRECTION('center_axis',(0.,1.,0.));
#28381=DIRECTION('ref_axis',(1.,0.,0.));
#28382=DIRECTION('center_axis',(0.,-1.,0.));
#28383=DIRECTION('ref_axis',(1.,0.,0.));
#28384=DIRECTION('center_axis',(0.,1.,0.));
#28385=DIRECTION('ref_axis',(1.,0.,-1.97812565634772E-16));
#28386=DIRECTION('',(0.,1.,0.));
#28387=DIRECTION('center_axis',(0.,-1.,0.));
#28388=DIRECTION('ref_axis',(1.,0.,-1.97812565634772E-16));
#28389=DIRECTION('center_axis',(1.,0.,0.));
#28390=DIRECTION('ref_axis',(0.,0.,-1.));
#28391=DIRECTION('',(0.,0.,-1.));
#28392=DIRECTION('center_axis',(0.,1.,0.));
#28393=DIRECTION('ref_axis',(1.,0.,0.));
#28394=DIRECTION('',(0.,1.,0.));
#28395=DIRECTION('center_axis',(0.,1.,0.));
#28396=DIRECTION('ref_axis',(1.,0.,0.));
#28397=DIRECTION('center_axis',(1.,0.,0.));
#28398=DIRECTION('ref_axis',(0.,0.,-1.));
#28399=DIRECTION('',(0.,0.,-1.));
#28400=DIRECTION('center_axis',(0.,1.,0.));
#28401=DIRECTION('ref_axis',(1.,0.,0.));
#28402=DIRECTION('center_axis',(0.,-1.,0.));
#28403=DIRECTION('ref_axis',(1.,0.,0.));
#28404=DIRECTION('',(0.,-1.,0.));
#28405=DIRECTION('center_axis',(0.,1.,0.));
#28406=DIRECTION('ref_axis',(1.,0.,0.));
#28407=DIRECTION('center_axis',(0.,1.,0.));
#28408=DIRECTION('ref_axis',(1.,0.,0.));
#28409=DIRECTION('',(0.,1.,0.));
#28410=DIRECTION('center_axis',(0.,1.,0.));
#28411=DIRECTION('ref_axis',(1.,0.,0.));
#28412=DIRECTION('center_axis',(0.,1.,0.));
#28413=DIRECTION('ref_axis',(1.,0.,0.));
#28414=DIRECTION('center_axis',(0.,1.,0.));
#28415=DIRECTION('ref_axis',(1.,0.,0.));
#28416=DIRECTION('',(0.,1.,0.));
#28417=DIRECTION('center_axis',(0.,1.,0.));
#28418=DIRECTION('ref_axis',(1.,0.,0.));
#28419=DIRECTION('center_axis',(0.,1.,0.));
#28420=DIRECTION('ref_axis',(1.,0.,0.));
#28421=DIRECTION('center_axis',(0.,-1.,0.));
#28422=DIRECTION('ref_axis',(1.,0.,0.));
#28423=DIRECTION('center_axis',(0.,-1.,0.));
#28424=DIRECTION('ref_axis',(1.,0.,0.));
#28425=DIRECTION('',(0.,-1.,0.));
#28426=DIRECTION('center_axis',(0.,-1.,0.));
#28427=DIRECTION('ref_axis',(1.,0.,0.));
#28428=DIRECTION('center_axis',(0.,-1.,0.));
#28429=DIRECTION('ref_axis',(1.,0.,0.));
#28430=DIRECTION('',(0.,-1.,0.));
#28431=DIRECTION('center_axis',(0.,-1.,0.));
#28432=DIRECTION('ref_axis',(1.,0.,0.));
#28433=DIRECTION('center_axis',(0.,-1.,0.));
#28434=DIRECTION('ref_axis',(1.,0.,0.));
#28435=DIRECTION('',(0.,-1.,0.));
#28436=DIRECTION('center_axis',(0.,-1.,0.));
#28437=DIRECTION('ref_axis',(1.,0.,0.));
#28438=DIRECTION('center_axis',(0.,-1.,0.));
#28439=DIRECTION('ref_axis',(1.,0.,0.));
#28440=DIRECTION('',(0.,-1.,0.));
#28441=DIRECTION('center_axis',(0.,1.,0.));
#28442=DIRECTION('ref_axis',(1.,0.,0.));
#28443=DIRECTION('center_axis',(0.,1.,0.));
#28444=DIRECTION('ref_axis',(1.,0.,0.));
#28445=DIRECTION('center_axis',(0.,1.,0.));
#28446=DIRECTION('ref_axis',(1.,0.,0.));
#28447=DIRECTION('center_axis',(0.,1.,0.));
#28448=DIRECTION('ref_axis',(1.,0.,0.));
#28449=DIRECTION('center_axis',(0.,1.,0.));
#28450=DIRECTION('ref_axis',(-4.44089209850063E-16,0.,1.));
#28451=DIRECTION('',(0.,1.,0.));
#28452=DIRECTION('center_axis',(0.,0.,1.));
#28453=DIRECTION('ref_axis',(1.,0.,0.));
#28454=DIRECTION('',(0.,1.,0.));
#28455=DIRECTION('center_axis',(0.,1.,0.));
#28456=DIRECTION('ref_axis',(-1.,0.,-8.88178419700126E-16));
#28457=DIRECTION('',(0.,1.,0.));
#28458=DIRECTION('center_axis',(-1.,0.,0.));
#28459=DIRECTION('ref_axis',(0.,0.,1.));
#28460=DIRECTION('axis',(0.,0.,1.));
#28461=DIRECTION('refdir',(1.,0.,0.));
#28462=DIRECTION('center_axis',(-0.548644247294728,-0.70710678118655,0.446082380183749));
#28463=DIRECTION('ref_axis',(0.630855751991531,0.,0.775900135442185));
#28464=DIRECTION('',(-0.228100862670962,-0.386714295024757,-0.893544654996195));
#28465=DIRECTION('',(0.630855751991531,0.,0.775900135442185));
#28466=DIRECTION('',(0.525361147399585,-0.706639907076674,-0.473978592902317));
#28467=DIRECTION('',(-0.630855751991531,0.,-0.775900135442185));
#28468=DIRECTION('',(-0.473949429076065,-0.176491388068498,-0.862683446355688));
#28469=DIRECTION('',(-0.327151215534528,-0.309436927624306,-0.892872258498779));
#28470=DIRECTION('center_axis',(0.,1.,0.));
#28471=DIRECTION('ref_axis',(1.,0.,0.));
#28472=DIRECTION('',(0.742482951693498,0.,-0.669864961350055));
#28473=DIRECTION('',(-0.247344359222329,0.,-0.968927638144818));
#28474=DIRECTION('',(-0.165201002238474,0.,-0.986259919523958));
#28475=DIRECTION('',(-0.0915937869476479,0.,-0.995796454197638));
#28476=DIRECTION('',(-0.0238849697840824,0.,-0.999714713414989));
#28477=DIRECTION('',(0.0393519680027076,0.,-0.99922541131334));
#28478=DIRECTION('',(0.0989820318029304,0.,-0.995089220813975));
#28479=DIRECTION('',(0.854702313102447,0.,-0.51911844118402));
#28480=DIRECTION('',(0.862298277386214,0.,-0.506400711706418));
#28481=DIRECTION('',(0.869705019525388,0.,-0.493571858002809));
#28482=DIRECTION('',(0.876920914189556,0.,-0.480634695228043));
#28483=DIRECTION('',(0.911263560158432,0.,0.411823656347446));
#28484=DIRECTION('',(0.885030574305658,0.,0.465532901677419));
#28485=DIRECTION('',(0.85383585346242,0.,0.520542347309132));
#28486=DIRECTION('',(0.816588132859797,0.,0.577220773424303));
#28487=DIRECTION('',(0.771525643922909,0.,0.636198224431145));
#28488=DIRECTION('',(0.715443769451104,0.,0.69867031764173));
#28489=DIRECTION('',(-0.356521352096954,0.,-0.934287175069293));
#28490=DIRECTION('',(0.951361549480978,0.,-0.308076617368395));
#28491=DIRECTION('',(0.977941578718451,0.,-0.20887859778748));
#28492=DIRECTION('',(0.158387039627108,0.,0.987377104088484));
#28493=DIRECTION('',(0.270257320503068,0.,-0.962788128673439));
#28494=DIRECTION('',(0.350061695092817,0.,-0.936726646161378));
#28495=DIRECTION('',(0.418575680773335,0.,-0.908181919807446));
#28496=DIRECTION('',(0.479172366105872,0.,-0.877720823246493));
#28497=DIRECTION('',(0.533692509635919,0.,-0.845678606302959));
#28498=DIRECTION('',(0.583265564466523,0.,-0.812281528355501));
#28499=DIRECTION('',(0.99975313641205,0.,-0.0222186010871085));
#28500=DIRECTION('',(0.999972569709231,0.,-0.00740674213917776));
#28501=DIRECTION('',(0.999972569709231,0.,0.00740674213917776));
#28502=DIRECTION('',(0.99975313641205,0.,0.0222186010871084));
#28503=DIRECTION('',(0.583265564466523,0.,0.812281528355501));
#28504=DIRECTION('',(0.533692509635919,0.,0.845678606302959));
#28505=DIRECTION('',(0.479172366105872,0.,0.877720823246493));
#28506=DIRECTION('',(0.418575680773335,0.,0.908181919807446));
#28507=DIRECTION('',(0.350061695092817,0.,0.936726646161378));
#28508=DIRECTION('',(0.270257320503068,0.,0.962788128673439));
#28509=DIRECTION('',(0.158387039627108,0.,-0.987377104088484));
#28510=DIRECTION('',(0.977941578718451,0.,0.208878597787478));
#28511=DIRECTION('',(0.951361549480978,0.,0.308076617368396));
#28512=DIRECTION('',(-0.356521352096954,0.,0.934287175069293));
#28513=DIRECTION('',(0.715443769451087,0.,-0.698670317641747));
#28514=DIRECTION('',(0.771525643922913,0.,-0.63619822443114));
#28515=DIRECTION('',(0.816588132859796,0.,-0.577220773424304));
#28516=DIRECTION('',(0.853835853462428,0.,-0.520542347309119));
#28517=DIRECTION('',(0.885030574305657,0.,-0.465532901677421));
#28518=DIRECTION('',(0.911263560158431,0.,-0.411823656347449));
#28519=DIRECTION('',(0.876920914189562,0.,0.480634695228032));
#28520=DIRECTION('',(0.869705019525386,0.,0.493571858002812));
#28521=DIRECTION('',(0.862298277386212,0.,0.506400711706423));
#28522=DIRECTION('',(0.85470231310245,0.,0.519118441184015));
#28523=DIRECTION('',(0.0989820318029246,0.,0.995089220813975));
#28524=DIRECTION('',(0.0393519680027008,0.,0.999225411313341));
#28525=DIRECTION('',(-0.0238849697840649,0.,0.999714713414989));
#28526=DIRECTION('',(-0.0915937869476482,0.,0.995796454197638));
#28527=DIRECTION('',(-0.165201002238466,0.,0.986259919523959));
#28528=DIRECTION('',(-0.247344359222354,0.,0.968927638144812));
#28529=DIRECTION('',(0.63085575199153,0.,-0.775900135442185));
#28530=DIRECTION('',(0.742482951693498,0.,0.669864961350055));
#28531=DIRECTION('',(0.669864961350055,0.,0.742482951693498));
#28532=DIRECTION('',(-0.775900135442185,0.,0.63085575199153));
#28533=DIRECTION('',(0.968927638144813,0.,-0.247344359222349));
#28534=DIRECTION('',(0.986259919523959,0.,-0.165201002238466));
#28535=DIRECTION('',(0.995796454197638,0.,-0.0915937869476553));
#28536=DIRECTION('',(0.999714713414989,0.,-0.0238849697840649));
#28537=DIRECTION('',(0.99922541131334,0.,0.039351968002701));
#28538=DIRECTION('',(0.995089220813975,0.,0.0989820318029272));
#28539=DIRECTION('',(0.519118441184011,0.,0.854702313102452));
#28540=DIRECTION('',(0.506400711706425,0.,0.862298277386211));
#28541=DIRECTION('',(0.493571858002802,0.,0.869705019525391));
#28542=DIRECTION('',(0.480634695228039,0.,0.876920914189558));
#28543=DIRECTION('',(-0.411823656347455,0.,0.911263560158428));
#28544=DIRECTION('',(-0.465532901677421,0.,0.885030574305657));
#28545=DIRECTION('',(-0.520542347309117,0.,0.853835853462429));
#28546=DIRECTION('',(-0.577220773424305,0.,0.816588132859795));
#28547=DIRECTION('',(-0.636198224431141,0.,0.771525643922912));
#28548=DIRECTION('',(-0.698670317641746,0.,0.715443769451088));
#28549=DIRECTION('',(0.934287175069293,0.,-0.356521352096954));
#28550=DIRECTION('',(0.308076617368396,0.,0.951361549480978));
#28551=DIRECTION('',(0.208878597787478,0.,0.977941578718451));
#28552=DIRECTION('',(-0.987377104088484,0.,0.158387039627108));
#28553=DIRECTION('',(0.962788128673439,0.,0.270257320503068));
#28554=DIRECTION('',(0.936726646161378,0.,0.350061695092817));
#28555=DIRECTION('',(0.908181919807447,0.,0.418575680773333));
#28556=DIRECTION('',(0.877720823246493,0.,0.479172366105871));
#28557=DIRECTION('',(0.845678606302959,0.,0.533692509635919));
#28558=DIRECTION('',(0.812281528355501,0.,0.583265564466523));
#28559=DIRECTION('',(0.0222186010871084,0.,0.99975313641205));
#28560=DIRECTION('',(0.00740674213917775,0.,0.999972569709231));
#28561=DIRECTION('',(-0.00740674213917775,0.,0.999972569709231));
#28562=DIRECTION('',(-0.0222186010871084,0.,0.99975313641205));
#28563=DIRECTION('',(-0.812281528355501,0.,0.583265564466523));
#28564=DIRECTION('',(-0.845678606302959,0.,0.533692509635919));
#28565=DIRECTION('',(-0.877720823246493,0.,0.479172366105871));
#28566=DIRECTION('',(-0.908181919807447,0.,0.418575680773333));
#28567=DIRECTION('',(-0.936726646161378,0.,0.350061695092817));
#28568=DIRECTION('',(-0.962788128673439,0.,0.270257320503068));
#28569=DIRECTION('',(0.987377104088484,0.,0.158387039627108));
#28570=DIRECTION('',(-0.208878597787478,0.,0.977941578718451));
#28571=DIRECTION('',(-0.308076617368396,0.,0.951361549480978));
#28572=DIRECTION('',(-0.934287175069293,0.,-0.356521352096954));
#28573=DIRECTION('',(0.698670317641746,0.,0.715443769451088));
#28574=DIRECTION('',(0.636198224431141,0.,0.771525643922912));
#28575=DIRECTION('',(0.577220773424305,0.,0.816588132859795));
#28576=DIRECTION('',(0.520542347309117,0.,0.853835853462429));
#28577=DIRECTION('',(0.465532901677421,0.,0.885030574305657));
#28578=DIRECTION('',(0.411823656347455,0.,0.911263560158428));
#28579=DIRECTION('',(-0.480634695228039,0.,0.876920914189558));
#28580=DIRECTION('',(-0.493571858002802,0.,0.869705019525391));
#28581=DIRECTION('',(-0.506400711706425,0.,0.862298277386211));
#28582=DIRECTION('',(-0.519118441184011,0.,0.854702313102452));
#28583=DIRECTION('',(-0.995089220813975,0.,0.0989820318029272));
#28584=DIRECTION('',(-0.99922541131334,0.,0.039351968002701));
#28585=DIRECTION('',(-0.999714713414989,0.,-0.0238849697840649));
#28586=DIRECTION('',(-0.995796454197638,0.,-0.0915937869476553));
#28587=DIRECTION('',(-0.986259919523959,0.,-0.165201002238466));
#28588=DIRECTION('',(-0.968927638144813,0.,-0.247344359222349));
#28589=DIRECTION('',(0.775900135442185,0.,0.63085575199153));
#28590=DIRECTION('',(-0.669864961350055,0.,0.742482951693498));
#28591=DIRECTION('',(-0.742482951693498,0.,0.669864961350055));
#28592=DIRECTION('',(-0.63085575199153,0.,-0.775900135442185));
#28593=DIRECTION('',(0.247344359222354,0.,0.968927638144812));
#28594=DIRECTION('',(0.165201002238466,0.,0.986259919523959));
#28595=DIRECTION('',(0.0915937869476482,0.,0.995796454197638));
#28596=DIRECTION('',(0.0238849697840649,0.,0.999714713414989));
#28597=DIRECTION('',(-0.0393519680027008,0.,0.999225411313341));
#28598=DIRECTION('',(-0.0989820318029246,0.,0.995089220813975));
#28599=DIRECTION('',(-0.85470231310245,0.,0.519118441184015));
#28600=DIRECTION('',(-0.862298277386212,0.,0.506400711706423));
#28601=DIRECTION('',(-0.869705019525386,0.,0.493571858002812));
#28602=DIRECTION('',(-0.876920914189562,0.,0.480634695228032));
#28603=DIRECTION('',(-0.911263560158431,0.,-0.411823656347449));
#28604=DIRECTION('',(-0.885030574305657,0.,-0.465532901677421));
#28605=DIRECTION('',(-0.853835853462428,0.,-0.520542347309119));
#28606=DIRECTION('',(-0.816588132859796,0.,-0.577220773424304));
#28607=DIRECTION('',(-0.771525643922913,0.,-0.63619822443114));
#28608=DIRECTION('',(-0.715443769451087,0.,-0.698670317641747));
#28609=DIRECTION('',(0.356521352096954,0.,0.934287175069293));
#28610=DIRECTION('',(-0.951361549480978,0.,0.308076617368396));
#28611=DIRECTION('',(-0.977941578718451,0.,0.208878597787478));
#28612=DIRECTION('',(-0.158387039627108,0.,-0.987377104088484));
#28613=DIRECTION('',(-0.270257320503068,0.,0.962788128673439));
#28614=DIRECTION('',(-0.350061695092817,0.,0.936726646161378));
#28615=DIRECTION('',(-0.418575680773335,0.,0.908181919807446));
#28616=DIRECTION('',(-0.479172366105872,0.,0.877720823246493));
#28617=DIRECTION('',(-0.533692509635919,0.,0.845678606302959));
#28618=DIRECTION('',(-0.583265564466523,0.,0.812281528355501));
#28619=DIRECTION('',(-0.99975313641205,0.,0.0222186010871084));
#28620=DIRECTION('',(-0.999972569709231,0.,0.00740674213917776));
#28621=DIRECTION('',(-0.999972569709231,0.,-0.00740674213917776));
#28622=DIRECTION('',(-0.99975313641205,0.,-0.0222186010871085));
#28623=DIRECTION('',(-0.583265564466523,0.,-0.812281528355501));
#28624=DIRECTION('',(-0.533692509635919,0.,-0.845678606302959));
#28625=DIRECTION('',(-0.479172366105872,0.,-0.877720823246493));
#28626=DIRECTION('',(-0.418575680773335,0.,-0.908181919807446));
#28627=DIRECTION('',(-0.350061695092817,0.,-0.936726646161378));
#28628=DIRECTION('',(-0.270257320503068,0.,-0.962788128673439));
#28629=DIRECTION('',(-0.158387039627108,0.,0.987377104088484));
#28630=DIRECTION('',(-0.977941578718451,0.,-0.208878597787479));
#28631=DIRECTION('',(-0.951361549480978,0.,-0.308076617368397));
#28632=DIRECTION('',(0.356521352096954,0.,-0.934287175069293));
#28633=DIRECTION('',(-0.715443769451089,0.,0.698670317641745));
#28634=DIRECTION('',(-0.771525643922911,0.,0.636198224431142));
#28635=DIRECTION('',(-0.816588132859795,0.,0.577220773424306));
#28636=DIRECTION('',(-0.853835853462428,0.,0.520542347309119));
#28637=DIRECTION('',(-0.885030574305657,0.,0.46553290167742));
#28638=DIRECTION('',(-0.911263560158429,0.,0.411823656347453));
#28639=DIRECTION('',(-0.876920914189557,0.,-0.48063469522804));
#28640=DIRECTION('',(-0.86970501952539,0.,-0.493571858002805));
#28641=DIRECTION('',(-0.86229827738621,0.,-0.506400711706427));
#28642=DIRECTION('',(-0.85470231310245,0.,-0.519118441184015));
#28643=DIRECTION('',(-0.0989820318029307,0.,-0.995089220813975));
#28644=DIRECTION('',(-0.0393519680026975,0.,-0.999225411313341));
#28645=DIRECTION('',(0.0238849697840614,0.,-0.99971471341499));
#28646=DIRECTION('',(0.0915937869476591,0.,-0.995796454197637));
#28647=DIRECTION('',(0.165201002238462,0.,-0.98625991952396));
#28648=DIRECTION('',(0.247344359222349,0.,-0.968927638144813));
#28649=DIRECTION('',(-0.63085575199153,0.,0.775900135442185));
#28650=DIRECTION('',(-0.742482951693498,0.,-0.669864961350055));
#28651=DIRECTION('',(-0.669864961350055,0.,-0.742482951693498));
#28652=DIRECTION('',(0.775900135442185,0.,-0.63085575199153));
#28653=DIRECTION('',(-0.968927638144812,0.,0.247344359222352));
#28654=DIRECTION('',(-0.98625991952396,0.,0.165201002238459));
#28655=DIRECTION('',(-0.995796454197637,0.,0.0915937869476627));
#28656=DIRECTION('',(-0.99971471341499,0.,0.0238849697840613));
#28657=DIRECTION('',(-0.999225411313341,0.,-0.0393519680026977));
#28658=DIRECTION('',(-0.995089220813975,0.,-0.0989820318029304));
#28659=DIRECTION('',(-0.519118441184006,0.,-0.854702313102456));
#28660=DIRECTION('',(-0.506400711706431,0.,-0.862298277386207));
#28661=DIRECTION('',(-0.493571858002802,0.,-0.869705019525391));
#28662=DIRECTION('',(-0.480634695228042,0.,-0.876920914189556));
#28663=DIRECTION('',(0.41182365634745,0.,-0.91126356015843));
#28664=DIRECTION('',(0.465532901677425,0.,-0.885030574305655));
#28665=DIRECTION('',(0.520542347309115,0.,-0.85383585346243));
#28666=DIRECTION('',(0.577220773424311,0.,-0.816588132859791));
#28667=DIRECTION('',(0.636198224431136,0.,-0.771525643922916));
#28668=DIRECTION('',(0.698670317641747,0.,-0.715443769451087));
#28669=DIRECTION('',(-0.934287175069293,0.,0.356521352096954));
#28670=DIRECTION('',(-0.308076617368396,0.,-0.951361549480978));
#28671=DIRECTION('',(-0.20887859778748,0.,-0.977941578718451));
#28672=DIRECTION('',(0.987377104088484,0.,-0.158387039627109));
#28673=DIRECTION('',(-0.962788128673439,0.,-0.270257320503066));
#28674=DIRECTION('',(-0.936726646161376,0.,-0.350061695092823));
#28675=DIRECTION('',(-0.908181919807451,0.,-0.418575680773325));
#28676=DIRECTION('',(-0.87772082324649,0.,-0.479172366105876));
#28677=DIRECTION('',(-0.84567860630296,0.,-0.533692509635917));
#28678=DIRECTION('',(-0.8122815283555,0.,-0.583265564466524));
#28679=DIRECTION('',(-0.0222186010871084,0.,-0.99975313641205));
#28680=DIRECTION('',(-0.00740674213917776,0.,-0.999972569709231));
#28681=DIRECTION('',(0.00740674213917776,0.,-0.999972569709231));
#28682=DIRECTION('',(0.0222186010871084,0.,-0.99975313641205));
#28683=DIRECTION('',(0.812281528355498,0.,-0.583265564466527));
#28684=DIRECTION('',(0.845678606302961,0.,-0.533692509635915));
#28685=DIRECTION('',(0.87772082324649,0.,-0.479172366105876));
#28686=DIRECTION('',(0.908181919807451,0.,-0.418575680773326));
#28687=DIRECTION('',(0.936726646161376,0.,-0.350061695092823));
#28688=DIRECTION('',(0.962788128673439,0.,-0.270257320503067));
#28689=DIRECTION('',(-0.987377104088484,0.,-0.158387039627108));
#28690=DIRECTION('',(0.208878597787478,0.,-0.977941578718451));
#28691=DIRECTION('',(0.308076617368396,0.,-0.951361549480978));
#28692=DIRECTION('',(0.934287175069293,0.,0.356521352096954));
#28693=DIRECTION('',(-0.69867031764175,0.,-0.715443769451084));
#28694=DIRECTION('',(-0.636198224431135,0.,-0.771525643922917));
#28695=DIRECTION('',(-0.577220773424313,0.,-0.81658813285979));
#28696=DIRECTION('',(-0.520542347309115,0.,-0.85383585346243));
#28697=DIRECTION('',(-0.465532901677422,0.,-0.885030574305656));
#28698=DIRECTION('',(-0.411823656347447,0.,-0.911263560158432));
#28699=DIRECTION('',(0.48063469522803,0.,-0.876920914189563));
#28700=DIRECTION('',(0.493571858002814,0.,-0.869705019525385));
#28701=DIRECTION('',(0.506400711706419,0.,-0.862298277386214));
#28702=DIRECTION('',(0.519118441184019,0.,-0.854702313102448));
#28703=DIRECTION('',(0.995089220813975,0.,-0.0989820318029307));
#28704=DIRECTION('',(0.999225411313341,0.,-0.0393519680026942));
#28705=DIRECTION('',(0.99971471341499,0.,0.023884969784058));
#28706=DIRECTION('',(0.995796454197637,0.,0.091593786947663));
#28707=DIRECTION('',(0.986259919523961,0.,0.165201002238458));
#28708=DIRECTION('',(0.968927638144812,0.,0.247344359222354));
#28709=DIRECTION('',(-0.775900135442185,0.,-0.630855751991531));
#28710=DIRECTION('',(0.669864961350053,0.,-0.742482951693499));
#28711=DIRECTION('center_axis',(0.,-1.,0.));
#28712=DIRECTION('ref_axis',(0.,0.,1.));
#28713=DIRECTION('center_axis',(-0.968927638144818,0.,0.247344359222329));
#28714=DIRECTION('ref_axis',(0.247344359222329,0.,0.968927638144818));
#28715=DIRECTION('',(0.,1.,0.));
#28716=DIRECTION('',(0.228100862670962,-0.386714295024757,0.893544654996195));
#28717=DIRECTION('',(0.247344359222329,0.,0.968927638144818));
#28718=DIRECTION('',(0.,1.,0.));
#28719=DIRECTION('center_axis',(-0.938956260693934,0.,0.344036539489144));
#28720=DIRECTION('ref_axis',(0.344036539489144,0.,0.938956260693934));
#28721=DIRECTION('',(0.,1.,0.));
#28722=DIRECTION('',(0.327151215534528,-0.309436927624306,0.892872258498779));
#28723=DIRECTION('center_axis',(-0.252098665705552,-0.707106781186548,0.660640797067119));
#28724=DIRECTION('ref_axis',(0.934287175069293,0.,0.356521352096954));
#28725=DIRECTION('',(-0.64431346919632,-0.386714295024737,-0.659781939307013));
#28726=DIRECTION('',(0.217986803358223,-0.706639907076675,-0.673158076003201));
#28727=DIRECTION('',(-0.934287175069293,0.,-0.356521352096954));
#28728=DIRECTION('',(-0.841793968866839,-0.176491388068509,-0.510131065430313));
#28729=DIRECTION('',(-0.729757392781244,-0.309436927624312,-0.609674450427068));
#28730=DIRECTION('center_axis',(-0.715443769451084,0.,0.69867031764175));
#28731=DIRECTION('ref_axis',(0.69867031764175,0.,0.715443769451084));
#28732=DIRECTION('',(0.,1.,0.));
#28733=DIRECTION('',(0.64431346919632,-0.386714295024737,0.659781939307013));
#28734=DIRECTION('',(0.69867031764175,0.,0.715443769451084));
#28735=DIRECTION('',(0.,1.,0.));
#28736=DIRECTION('center_axis',(-0.641141705058825,0.,0.767422513374649));
#28737=DIRECTION('ref_axis',(0.767422513374649,0.,0.641141705058824));
#28738=DIRECTION('',(0.,1.,0.));
#28739=DIRECTION('',(0.729757392781244,-0.309436927624312,0.609674450427068));
#28740=DIRECTION('center_axis',(0.111996549772391,-0.707106781186548,0.698181045889302));
#28741=DIRECTION('ref_axis',(0.987377104088484,0.,-0.158387039627109));
#28742=DIRECTION('',(-0.887882801977999,-0.386714295024741,-0.24923118579988));
#28743=DIRECTION('',(-0.147796928603617,-0.706639907076676,-0.691965396260539));
#28744=DIRECTION('',(-0.987377104088484,0.,0.158387039627109));
#28745=DIRECTION('',(-0.984080494506366,-0.176491388068509,-0.0208894774888531));
#28746=DIRECTION('',(-0.936825665961593,-0.309436927624307,-0.16311486571753));
#28747=DIRECTION('center_axis',(-0.270257320503066,0.,0.962788128673439));
#28748=DIRECTION('ref_axis',(0.962788128673439,0.,0.270257320503066));
#28749=DIRECTION('',(0.,1.,0.));
#28750=DIRECTION('',(0.887882801977999,-0.386714295024741,0.24923118579988));
#28751=DIRECTION('',(0.962788128673439,0.,0.270257320503066));
#28752=DIRECTION('',(0.,1.,0.));
#28753=DIRECTION('center_axis',(-0.171533747319281,0.,0.985178244547963));
#28754=DIRECTION('ref_axis',(0.985178244547962,0.,0.171533747319281));
#28755=DIRECTION('',(0.,1.,0.));
#28756=DIRECTION('',(0.936825665961593,-0.309436927624307,0.16311486571753));
#28757=DIRECTION('center_axis',(0.446082380183749,-0.70710678118655,0.548644247294728));
#28758=DIRECTION('ref_axis',(0.775900135442185,0.,-0.63085575199153));
#28759=DIRECTION('',(-0.893544654996196,-0.386714295024739,0.228100862670985));
#28760=DIRECTION('',(-0.473978592902318,-0.706639907076674,-0.525361147399585));
#28761=DIRECTION('',(-0.775900135442185,0.,0.63085575199153));
#28762=DIRECTION('',(-0.862683446355692,-0.176491388068509,0.473949429076052));
#28763=DIRECTION('',(-0.892872258498779,-0.309436927624306,0.327151215534528));
#28764=DIRECTION('center_axis',(0.247344359222352,0.,0.968927638144812));
#28765=DIRECTION('ref_axis',(0.968927638144812,0.,-0.247344359222352));
#28766=DIRECTION('',(0.,1.,0.));
#28767=DIRECTION('',(0.893544654996196,-0.386714295024739,-0.228100862670985));
#28768=DIRECTION('',(0.968927638144812,0.,-0.247344359222352));
#28769=DIRECTION('',(0.,1.,0.));
#28770=DIRECTION('center_axis',(0.344036539489143,0.,0.938956260693934));
#28771=DIRECTION('ref_axis',(0.938956260693934,0.,-0.344036539489143));
#28772=DIRECTION('',(0.,1.,0.));
#28773=DIRECTION('',(0.892872258498779,-0.309436927624306,-0.327151215534528));
#28774=DIRECTION('center_axis',(0.660640797067119,-0.707106781186549,0.252098665705552));
#28775=DIRECTION('ref_axis',(0.356521352096954,0.,-0.934287175069293));
#28776=DIRECTION('',(-0.659781939307016,-0.386714295024741,0.644313469196315));
#28777=DIRECTION('',(-0.673158076003201,-0.706639907076675,-0.217986803358224));
#28778=DIRECTION('',(-0.356521352096954,0.,0.934287175069293));
#28779=DIRECTION('',(-0.510131065430304,-0.176491388068498,0.841793968866847));
#28780=DIRECTION('',(-0.609674450427068,-0.309436927624311,0.729757392781245));
#28781=DIRECTION('center_axis',(0.698670317641745,0.,0.715443769451089));
#28782=DIRECTION('ref_axis',(0.715443769451089,0.,-0.698670317641745));
#28783=DIRECTION('',(0.,1.,0.));
#28784=DIRECTION('',(0.659781939307016,-0.386714295024741,-0.644313469196315));
#28785=DIRECTION('',(0.715443769451089,0.,-0.698670317641745));
#28786=DIRECTION('',(0.,1.,0.));
#28787=DIRECTION('center_axis',(0.76742251337465,0.,0.641141705058824));
#28788=DIRECTION('ref_axis',(0.641141705058824,0.,-0.76742251337465));
#28789=DIRECTION('',(0.,1.,0.));
#28790=DIRECTION('',(0.609674450427068,-0.309436927624311,-0.729757392781245));
#28791=DIRECTION('center_axis',(0.698181045889302,-0.707106781186549,-0.11199654977239));
#28792=DIRECTION('ref_axis',(-0.158387039627108,0.,-0.987377104088484));
#28793=DIRECTION('',(-0.249231185799881,-0.386714295024742,0.887882801977999));
#28794=DIRECTION('',(-0.691965396260539,-0.706639907076675,0.147796928603616));
#28795=DIRECTION('',(0.158387039627108,0.,0.987377104088484));
#28796=DIRECTION('',(-0.0208894774888416,-0.176491388068498,0.984080494506368));
#28797=DIRECTION('',(-0.163114865717534,-0.309436927624311,0.936825665961591));
#28798=DIRECTION('center_axis',(0.962788128673439,0.,0.270257320503068));
#28799=DIRECTION('ref_axis',(0.270257320503068,0.,-0.962788128673439));
#28800=DIRECTION('',(0.,1.,0.));
#28801=DIRECTION('',(0.249231185799881,-0.386714295024742,-0.887882801977999));
#28802=DIRECTION('',(0.270257320503068,0.,-0.962788128673439));
#28803=DIRECTION('',(0.,1.,0.));
#28804=DIRECTION('center_axis',(0.985178244547962,0.,0.171533747319286));
#28805=DIRECTION('ref_axis',(0.171533747319286,0.,-0.985178244547962));
#28806=DIRECTION('',(0.,1.,0.));
#28807=DIRECTION('',(0.163114865717534,-0.309436927624311,-0.936825665961591));
#28808=DIRECTION('center_axis',(0.548644247294728,-0.70710678118655,-0.446082380183749));
#28809=DIRECTION('ref_axis',(-0.63085575199153,0.,-0.775900135442185));
#28810=DIRECTION('',(0.228100862670987,-0.386714295024738,0.893544654996197));
#28811=DIRECTION('',(-0.525361147399585,-0.706639907076674,0.473978592902318));
#28812=DIRECTION('',(0.63085575199153,0.,0.775900135442185));
#28813=DIRECTION('',(0.473949429076065,-0.176491388068497,0.862683446355688));
#28814=DIRECTION('',(0.327151215534519,-0.309436927624313,0.89287225849878));
#28815=DIRECTION('center_axis',(0.968927638144812,0.,-0.247344359222354));
#28816=DIRECTION('ref_axis',(-0.247344359222354,0.,-0.968927638144812));
#28817=DIRECTION('',(0.,1.,0.));
#28818=DIRECTION('',(-0.228100862670987,-0.386714295024738,-0.893544654996197));
#28819=DIRECTION('',(-0.247344359222354,0.,-0.968927638144812));
#28820=DIRECTION('',(0.,1.,0.));
#28821=DIRECTION('center_axis',(0.938956260693937,0.,-0.344036539489135));
#28822=DIRECTION('ref_axis',(-0.344036539489135,0.,-0.938956260693937));
#28823=DIRECTION('',(0.,1.,0.));
#28824=DIRECTION('',(-0.327151215534519,-0.309436927624313,-0.89287225849878));
#28825=DIRECTION('center_axis',(0.252098665705552,-0.707106781186548,-0.660640797067119));
#28826=DIRECTION('ref_axis',(-0.934287175069293,0.,-0.356521352096954));
#28827=DIRECTION('',(0.644313469196316,-0.386714295024741,0.659781939307015));
#28828=DIRECTION('',(-0.217986803358223,-0.706639907076675,0.673158076003201));
#28829=DIRECTION('',(0.934287175069293,0.,0.356521352096954));
#28830=DIRECTION('',(0.841793968866845,-0.1764913880685,0.510131065430306));
#28831=DIRECTION('',(0.729757392781242,-0.309436927624314,0.609674450427069));
#28832=DIRECTION('center_axis',(0.715443769451088,0.,-0.698670317641746));
#28833=DIRECTION('ref_axis',(-0.698670317641746,0.,-0.715443769451088));
#28834=DIRECTION('',(0.,1.,0.));
#28835=DIRECTION('',(-0.644313469196316,-0.386714295024741,-0.659781939307015));
#28836=DIRECTION('',(-0.698670317641746,0.,-0.715443769451088));
#28837=DIRECTION('',(0.,1.,0.));
#28838=DIRECTION('center_axis',(0.641141705058826,0.,-0.767422513374648));
#28839=DIRECTION('ref_axis',(-0.767422513374648,0.,-0.641141705058826));
#28840=DIRECTION('',(0.,1.,0.));
#28841=DIRECTION('',(-0.729757392781242,-0.309436927624314,-0.609674450427069));
#28842=DIRECTION('center_axis',(-0.11199654977239,-0.707106781186549,-0.698181045889302));
#28843=DIRECTION('ref_axis',(-0.987377104088484,0.,0.158387039627108));
#28844=DIRECTION('',(0.887882801977998,-0.386714295024742,0.249231185799882));
#28845=DIRECTION('',(0.147796928603616,-0.706639907076675,0.691965396260539));
#28846=DIRECTION('',(0.987377104088484,0.,-0.158387039627108));
#28847=DIRECTION('',(0.984080494506367,-0.176491388068501,0.0208894774888451));
#28848=DIRECTION('',(0.936825665961591,-0.309436927624309,0.163114865717533));
#28849=DIRECTION('center_axis',(0.270257320503069,0.,-0.962788128673439));
#28850=DIRECTION('ref_axis',(-0.962788128673439,0.,-0.270257320503069));
#28851=DIRECTION('',(0.,1.,0.));
#28852=DIRECTION('',(-0.887882801977998,-0.386714295024742,-0.249231185799882));
#28853=DIRECTION('',(-0.962788128673439,0.,-0.270257320503068));
#28854=DIRECTION('',(0.,1.,0.));
#28855=DIRECTION('center_axis',(0.171533747319284,0.,-0.985178244547962));
#28856=DIRECTION('ref_axis',(-0.985178244547962,0.,-0.171533747319284));
#28857=DIRECTION('',(0.,1.,0.));
#28858=DIRECTION('',(-0.936825665961591,-0.309436927624309,-0.163114865717533));
#28859=DIRECTION('center_axis',(-0.446082380183748,-0.707106781186549,-0.548644247294729));
#28860=DIRECTION('ref_axis',(-0.775900135442186,0.,0.63085575199153));
#28861=DIRECTION('',(0.893544654996196,-0.386714295024742,-0.228100862670982));
#28862=DIRECTION('',(0.473978592902317,-0.706639907076675,0.525361147399585));
#28863=DIRECTION('',(0.775900135442185,0.,-0.63085575199153));
#28864=DIRECTION('',(0.862683446355689,-0.176491388068498,-0.473949429076063));
#28865=DIRECTION('',(0.89287225849878,-0.30943692762431,-0.327151215534523));
#28866=DIRECTION('center_axis',(-0.247344359222349,0.,-0.968927638144813));
#28867=DIRECTION('ref_axis',(-0.968927638144813,0.,0.247344359222349));
#28868=DIRECTION('',(0.,1.,0.));
#28869=DIRECTION('',(-0.893544654996196,-0.386714295024742,0.228100862670982));
#28870=DIRECTION('',(-0.968927638144813,0.,0.247344359222349));
#28871=DIRECTION('',(0.,1.,0.));
#28872=DIRECTION('center_axis',(-0.344036539489138,0.,-0.938956260693936));
#28873=DIRECTION('ref_axis',(-0.938956260693936,0.,0.344036539489138));
#28874=DIRECTION('',(0.,1.,0.));
#28875=DIRECTION('',(-0.89287225849878,-0.30943692762431,0.327151215534523));
#28876=DIRECTION('center_axis',(-0.660640797067119,-0.707106781186548,-0.252098665705553));
#28877=DIRECTION('ref_axis',(-0.356521352096954,0.,0.934287175069293));
#28878=DIRECTION('',(0.659781939307015,-0.386714295024739,-0.644313469196317));
#28879=DIRECTION('',(0.673158076003201,-0.706639907076675,0.217986803358222));
#28880=DIRECTION('',(0.356521352096954,0.,-0.934287175069293));
#28881=DIRECTION('',(0.510131065430303,-0.176491388068496,-0.841793968866848));
#28882=DIRECTION('',(0.60967445042707,-0.309436927624314,-0.729757392781241));
#28883=DIRECTION('center_axis',(-0.698670317641747,0.,-0.715443769451087));
#28884=DIRECTION('ref_axis',(-0.715443769451087,0.,0.698670317641747));
#28885=DIRECTION('',(0.,1.,0.));
#28886=DIRECTION('',(-0.659781939307015,-0.386714295024739,0.644313469196317));
#28887=DIRECTION('',(-0.715443769451087,0.,0.698670317641747));
#28888=DIRECTION('',(0.,1.,0.));
#28889=DIRECTION('center_axis',(-0.767422513374647,0.,-0.641141705058827));
#28890=DIRECTION('ref_axis',(-0.641141705058827,0.,0.767422513374647));
#28891=DIRECTION('',(0.,1.,0.));
#28892=DIRECTION('',(-0.60967445042707,-0.309436927624314,0.729757392781241));
#28893=DIRECTION('center_axis',(-0.698181045889302,-0.707106781186549,0.111996549772391));
#28894=DIRECTION('ref_axis',(0.158387039627108,0.,0.987377104088484));
#28895=DIRECTION('',(0.249231185799882,-0.386714295024742,-0.887882801977999));
#28896=DIRECTION('',(0.691965396260539,-0.706639907076675,-0.147796928603617));
#28897=DIRECTION('',(-0.158387039627108,0.,-0.987377104088484));
#28898=DIRECTION('',(0.0208894774888421,-0.176491388068498,-0.984080494506368));
#28899=DIRECTION('',(0.163114865717534,-0.309436927624311,-0.936825665961591));
#28900=DIRECTION('center_axis',(-0.962788128673439,0.,-0.270257320503068));
#28901=DIRECTION('ref_axis',(-0.270257320503068,0.,0.962788128673439));
#28902=DIRECTION('',(0.,1.,0.));
#28903=DIRECTION('',(-0.249231185799882,-0.386714295024742,0.887882801977999));
#28904=DIRECTION('',(-0.270257320503068,0.,0.962788128673439));
#28905=DIRECTION('',(0.,1.,0.));
#28906=DIRECTION('center_axis',(-0.985178244547962,0.,-0.171533747319286));
#28907=DIRECTION('ref_axis',(-0.171533747319286,0.,0.985178244547962));
#28908=DIRECTION('',(0.,1.,0.));
#28909=DIRECTION('',(-0.163114865717534,-0.309436927624311,0.936825665961591));
#28910=DIRECTION('center_axis',(0.660640797067119,-0.707106781186549,-0.252098665705553));
#28911=DIRECTION('ref_axis',(-0.356521352096954,0.,-0.934287175069293));
#28912=DIRECTION('',(0.510131065430303,0.176491388068496,0.841793968866848));
#28913=DIRECTION('',(0.356521352096954,0.,0.934287175069293));
#28914=DIRECTION('',(0.673158076003201,0.706639907076675,-0.217986803358222));
#28915=DIRECTION('',(0.659781939307025,0.386714295024756,0.644313469196296));
#28916=DIRECTION('',(0.609674450427067,0.309436927624308,0.729757392781247));
#28917=DIRECTION('center_axis',(0.934287175069293,0.,-0.356521352096954));
#28918=DIRECTION('ref_axis',(-0.356521352096954,0.,-0.934287175069293));
#28919=DIRECTION('',(0.,1.,0.));
#28920=DIRECTION('',(-0.356521352096954,0.,-0.934287175069293));
#28921=DIRECTION('',(0.,1.,0.));
#28922=DIRECTION('center_axis',(0.855219039771101,0.,-0.518266720919833));
#28923=DIRECTION('ref_axis',(-0.518266720919833,0.,-0.855219039771101));
#28924=DIRECTION('',(0.,1.,0.));
#28925=DIRECTION('',(-0.510131065430303,0.176491388068496,-0.841793968866848));
#28926=DIRECTION('center_axis',(0.446082380183749,-0.70710678118655,-0.548644247294728));
#28927=DIRECTION('ref_axis',(-0.775900135442185,0.,-0.630855751991531));
#28928=DIRECTION('',(0.862683446355692,0.176491388068508,0.473949429076054));
#28929=DIRECTION('',(0.775900135442185,0.,0.630855751991531));
#28930=DIRECTION('',(0.473978592902316,0.706639907076674,-0.525361147399586));
#28931=DIRECTION('',(0.893544654996196,0.386714295024738,0.228100862670987));
#28932=DIRECTION('',(0.892872258498779,0.309436927624308,0.327151215534526));
#28933=DIRECTION('center_axis',(0.630855751991531,0.,-0.775900135442185));
#28934=DIRECTION('ref_axis',(-0.775900135442185,0.,-0.630855751991531));
#28935=DIRECTION('',(0.,1.,0.));
#28936=DIRECTION('',(-0.775900135442185,0.,-0.630855751991531));
#28937=DIRECTION('',(0.,1.,0.));
#28938=DIRECTION('center_axis',(0.481508053781981,0.,-0.876441666138191));
#28939=DIRECTION('ref_axis',(-0.876441666138191,0.,-0.481508053781981));
#28940=DIRECTION('',(0.,1.,0.));
#28941=DIRECTION('',(-0.862683446355692,0.176491388068508,-0.473949429076054));
#28942=DIRECTION('center_axis',(0.11199654977239,-0.707106781186549,-0.698181045889302));
#28943=DIRECTION('ref_axis',(-0.987377104088484,0.,-0.158387039627108));
#28944=DIRECTION('',(0.984080494506366,0.17649138806851,-0.020889477488854));
#28945=DIRECTION('',(0.987377104088484,0.,0.158387039627108));
#28946=DIRECTION('',(0.147796928603616,0.706639907076675,-0.691965396260539));
#28947=DIRECTION('',(0.887882801977999,0.386714295024741,-0.249231185799881));
#28948=DIRECTION('',(0.936825665961593,0.309436927624307,-0.16311486571753));
#28949=DIRECTION('center_axis',(0.158387039627108,0.,-0.987377104088484));
#28950=DIRECTION('ref_axis',(-0.987377104088484,0.,-0.158387039627108));
#28951=DIRECTION('',(0.,1.,0.));
#28952=DIRECTION('',(-0.987377104088484,0.,-0.158387039627108));
#28953=DIRECTION('',(0.,1.,0.));
#28954=DIRECTION('center_axis',(-0.0212226263670982,0.,-0.999774774701824));
#28955=DIRECTION('ref_axis',(-0.999774774701824,0.,0.0212226263670982));
#28956=DIRECTION('',(0.,1.,0.));
#28957=DIRECTION('',(-0.984080494506366,0.17649138806851,0.020889477488854));
#28958=DIRECTION('center_axis',(-0.252098665705553,-0.707106781186548,-0.66064079706712));
#28959=DIRECTION('ref_axis',(-0.934287175069293,0.,0.356521352096954));
#28960=DIRECTION('',(0.84179396886684,0.176491388068507,-0.510131065430311));
#28961=DIRECTION('',(0.934287175069293,0.,-0.356521352096954));
#28962=DIRECTION('',(-0.217986803358222,0.706639907076676,-0.6731580760032));
#28963=DIRECTION('',(0.644313469196317,0.38671429502474,-0.659781939307015));
#28964=DIRECTION('',(0.729757392781247,0.309436927624309,-0.609674450427066));
#28965=DIRECTION('center_axis',(-0.356521352096954,0.,-0.934287175069293));
#28966=DIRECTION('ref_axis',(-0.934287175069293,0.,0.356521352096954));
#28967=DIRECTION('',(0.,1.,0.));
#28968=DIRECTION('',(-0.934287175069293,0.,0.356521352096954));
#28969=DIRECTION('',(0.,1.,0.));
#28970=DIRECTION('center_axis',(-0.518266720919842,0.,-0.855219039771096));
#28971=DIRECTION('ref_axis',(-0.855219039771096,0.,0.518266720919842));
#28972=DIRECTION('',(0.,1.,0.));
#28973=DIRECTION('',(-0.84179396886684,0.176491388068507,0.510131065430311));
#28974=DIRECTION('center_axis',(-0.54864424729473,-0.707106781186548,-0.446082380183749));
#28975=DIRECTION('ref_axis',(-0.63085575199153,0.,0.775900135442186));
#28976=DIRECTION('',(0.473949429076053,0.176491388068509,-0.862683446355692));
#28977=DIRECTION('',(0.63085575199153,0.,-0.775900135442185));
#28978=DIRECTION('',(-0.525361147399584,0.706639907076676,-0.473978592902316));
#28979=DIRECTION('',(0.228100862670983,0.386714295024742,-0.893544654996196));
#28980=DIRECTION('',(0.327151215534528,0.309436927624306,-0.892872258498779));
#28981=DIRECTION('center_axis',(-0.775900135442186,0.,-0.63085575199153));
#28982=DIRECTION('ref_axis',(-0.63085575199153,0.,0.775900135442185));
#28983=DIRECTION('',(0.,1.,0.));
#28984=DIRECTION('',(-0.63085575199153,0.,0.775900135442185));
#28985=DIRECTION('',(0.,1.,0.));
#28986=DIRECTION('center_axis',(-0.876441666138192,0.,-0.48150805378198));
#28987=DIRECTION('ref_axis',(-0.48150805378198,0.,0.876441666138192));
#28988=DIRECTION('',(0.,1.,0.));
#28989=DIRECTION('',(-0.473949429076053,0.176491388068509,0.862683446355692));
#28990=DIRECTION('center_axis',(-0.698181045889302,-0.707106781186549,-0.111996549772391));
#28991=DIRECTION('ref_axis',(-0.158387039627108,0.,0.987377104088484));
#28992=DIRECTION('',(-0.0208894774888421,0.176491388068498,-0.984080494506368));
#28993=DIRECTION('',(0.158387039627108,0.,-0.987377104088484));
#28994=DIRECTION('',(-0.691965396260539,0.706639907076675,-0.147796928603617));
#28995=DIRECTION('',(-0.249231185799882,0.386714295024742,-0.887882801977999));
#28996=DIRECTION('',(-0.163114865717534,0.309436927624311,-0.936825665961591));
#28997=DIRECTION('center_axis',(-0.987377104088484,0.,-0.158387039627108));
#28998=DIRECTION('ref_axis',(-0.158387039627108,0.,0.987377104088484));
#28999=DIRECTION('',(0.,1.,0.));
#29000=DIRECTION('',(-0.158387039627108,0.,0.987377104088484));
#29001=DIRECTION('',(0.,1.,0.));
#29002=DIRECTION('center_axis',(-0.999774774701824,0.,0.0212226263670861));
#29003=DIRECTION('ref_axis',(0.0212226263670861,0.,0.999774774701824));
#29004=DIRECTION('',(0.,1.,0.));
#29005=DIRECTION('',(0.0208894774888421,0.176491388068498,0.984080494506368));
#29006=DIRECTION('center_axis',(-0.66064079706712,-0.707106781186548,0.252098665705553));
#29007=DIRECTION('ref_axis',(0.356521352096954,0.,0.934287175069293));
#29008=DIRECTION('',(-0.510131065430303,0.176491388068496,-0.841793968866848));
#29009=DIRECTION('',(-0.356521352096954,0.,-0.934287175069293));
#29010=DIRECTION('',(-0.673158076003201,0.706639907076676,0.217986803358222));
#29011=DIRECTION('',(-0.659781939307015,0.38671429502474,-0.644313469196317));
#29012=DIRECTION('',(-0.60967445042707,0.309436927624314,-0.729757392781241));
#29013=DIRECTION('center_axis',(-0.934287175069293,0.,0.356521352096954));
#29014=DIRECTION('ref_axis',(0.356521352096954,0.,0.934287175069293));
#29015=DIRECTION('',(0.,1.,0.));
#29016=DIRECTION('',(0.356521352096954,0.,0.934287175069293));
#29017=DIRECTION('',(0.,1.,0.));
#29018=DIRECTION('center_axis',(-0.855219039771101,0.,0.518266720919832));
#29019=DIRECTION('ref_axis',(0.518266720919832,0.,0.855219039771102));
#29020=DIRECTION('',(0.,1.,0.));
#29021=DIRECTION('',(0.510131065430303,0.176491388068496,0.841793968866848));
#29022=DIRECTION('center_axis',(-0.446082380183749,-0.707106781186548,0.54864424729473));
#29023=DIRECTION('ref_axis',(0.775900135442186,0.,0.63085575199153));
#29024=DIRECTION('',(-0.862683446355689,0.176491388068498,-0.473949429076063));
#29025=DIRECTION('',(-0.775900135442185,0.,-0.63085575199153));
#29026=DIRECTION('',(-0.473978592902316,0.706639907076676,0.525361147399584));
#29027=DIRECTION('',(-0.893544654996196,0.386714295024742,-0.228100862670982));
#29028=DIRECTION('',(-0.89287225849878,0.30943692762431,-0.327151215534523));
#29029=DIRECTION('center_axis',(-0.63085575199153,0.,0.775900135442186));
#29030=DIRECTION('ref_axis',(0.775900135442185,0.,0.63085575199153));
#29031=DIRECTION('',(0.,1.,0.));
#29032=DIRECTION('',(0.775900135442185,0.,0.63085575199153));
#29033=DIRECTION('',(0.,1.,0.));
#29034=DIRECTION('center_axis',(-0.481508053781989,0.,0.876441666138187));
#29035=DIRECTION('ref_axis',(0.876441666138187,0.,0.481508053781989));
#29036=DIRECTION('',(0.,1.,0.));
#29037=DIRECTION('',(0.862683446355689,0.176491388068498,0.473949429076063));
#29038=DIRECTION('center_axis',(-0.11199654977239,-0.707106781186549,0.698181045889302));
#29039=DIRECTION('ref_axis',(0.987377104088484,0.,0.158387039627108));
#29040=DIRECTION('',(-0.984080494506367,0.176491388068501,0.0208894774888451));
#29041=DIRECTION('',(-0.987377104088484,0.,-0.158387039627108));
#29042=DIRECTION('',(-0.147796928603616,0.706639907076675,0.69196539626054));
#29043=DIRECTION('',(-0.887882801977998,0.386714295024742,0.249231185799882));
#29044=DIRECTION('',(-0.936825665961591,0.309436927624309,0.163114865717533));
#29045=DIRECTION('center_axis',(-0.158387039627108,0.,0.987377104088484));
#29046=DIRECTION('ref_axis',(0.987377104088484,0.,0.158387039627108));
#29047=DIRECTION('',(0.,1.,0.));
#29048=DIRECTION('',(0.987377104088484,0.,0.158387039627108));
#29049=DIRECTION('',(0.,1.,0.));
#29050=DIRECTION('center_axis',(0.0212226263670891,0.,0.999774774701824));
#29051=DIRECTION('ref_axis',(0.999774774701824,0.,-0.0212226263670891));
#29052=DIRECTION('',(0.,1.,0.));
#29053=DIRECTION('',(0.984080494506367,0.176491388068501,-0.0208894774888451));
#29054=DIRECTION('center_axis',(0.252098665705552,-0.707106781186548,0.66064079706712));
#29055=DIRECTION('ref_axis',(0.934287175069293,0.,-0.356521352096954));
#29056=DIRECTION('',(-0.841793968866845,0.1764913880685,0.510131065430306));
#29057=DIRECTION('',(-0.934287175069293,0.,0.356521352096954));
#29058=DIRECTION('',(0.217986803358223,0.706639907076676,0.673158076003201));
#29059=DIRECTION('',(-0.644313469196316,0.386714295024741,0.659781939307015));
#29060=DIRECTION('',(-0.729757392781242,0.309436927624314,0.609674450427069));
#29061=DIRECTION('center_axis',(0.356521352096954,0.,0.934287175069293));
#29062=DIRECTION('ref_axis',(0.934287175069293,0.,-0.356521352096954));
#29063=DIRECTION('',(0.,1.,0.));
#29064=DIRECTION('',(0.934287175069293,0.,-0.356521352096954));
#29065=DIRECTION('',(0.,1.,0.));
#29066=DIRECTION('center_axis',(0.518266720919835,0.,0.855219039771099));
#29067=DIRECTION('ref_axis',(0.855219039771099,0.,-0.518266720919835));
#29068=DIRECTION('',(0.,1.,0.));
#29069=DIRECTION('',(0.841793968866845,0.1764913880685,-0.510131065430306));
#29070=DIRECTION('center_axis',(0.548644247294729,-0.707106781186549,0.446082380183749));
#29071=DIRECTION('ref_axis',(0.63085575199153,0.,-0.775900135442185));
#29072=DIRECTION('',(-0.473949429076064,0.176491388068498,0.862683446355688));
#29073=DIRECTION('',(-0.63085575199153,0.,0.775900135442185));
#29074=DIRECTION('',(0.525361147399584,0.706639907076675,0.473978592902317));
#29075=DIRECTION('',(-0.228100862670987,0.386714295024739,0.893544654996196));
#29076=DIRECTION('',(-0.327151215534519,0.309436927624314,0.89287225849878));
#29077=DIRECTION('center_axis',(0.775900135442185,0.,0.630855751991531));
#29078=DIRECTION('ref_axis',(0.63085575199153,0.,-0.775900135442185));
#29079=DIRECTION('',(0.,1.,0.));
#29080=DIRECTION('',(0.63085575199153,0.,-0.775900135442185));
#29081=DIRECTION('',(0.,1.,0.));
#29082=DIRECTION('center_axis',(0.876441666138186,0.,0.481508053781991));
#29083=DIRECTION('ref_axis',(0.481508053781991,0.,-0.876441666138186));
#29084=DIRECTION('',(0.,1.,0.));
#29085=DIRECTION('',(0.473949429076064,0.176491388068498,-0.862683446355688));
#29086=DIRECTION('center_axis',(0.698181045889302,-0.707106781186549,0.11199654977239));
#29087=DIRECTION('ref_axis',(0.158387039627108,0.,-0.987377104088484));
#29088=DIRECTION('',(0.0208894774888416,0.176491388068498,0.984080494506368));
#29089=DIRECTION('',(-0.158387039627108,0.,0.987377104088484));
#29090=DIRECTION('',(0.69196539626054,0.706639907076675,0.147796928603616));
#29091=DIRECTION('',(0.249231185799881,0.386714295024741,0.887882801977999));
#29092=DIRECTION('',(0.163114865717534,0.309436927624311,0.936825665961591));
#29093=DIRECTION('center_axis',(0.987377104088484,0.,0.158387039627108));
#29094=DIRECTION('ref_axis',(0.158387039627108,0.,-0.987377104088484));
#29095=DIRECTION('',(0.,1.,0.));
#29096=DIRECTION('',(0.158387039627108,0.,-0.987377104088484));
#29097=DIRECTION('',(0.,1.,0.));
#29098=DIRECTION('center_axis',(0.999774774701824,0.,-0.0212226263670855));
#29099=DIRECTION('ref_axis',(-0.0212226263670855,0.,-0.999774774701824));
#29100=DIRECTION('',(0.,1.,0.));
#29101=DIRECTION('',(-0.0208894774888416,0.176491388068498,-0.984080494506368));
#29102=DIRECTION('center_axis',(-0.698181045889302,0.707106781186549,0.111996549772391));
#29103=DIRECTION('ref_axis',(0.158387039627108,0.,0.987377104088484));
#29104=DIRECTION('',(-0.0208894774888421,-0.176491388068498,0.984080494506368));
#29105=DIRECTION('',(0.158387039627108,0.,0.987377104088484));
#29106=DIRECTION('',(-0.691965396260539,-0.706639907076675,0.147796928603617));
#29107=DIRECTION('',(-0.158387039627108,0.,-0.987377104088484));
#29108=DIRECTION('center_axis',(0.,1.,0.));
#29109=DIRECTION('ref_axis',(0.,0.,1.));
#29110=DIRECTION('',(-0.977941578718451,0.,0.20887859778748));
#29111=DIRECTION('',(-0.951361549480978,0.,0.308076617368395));
#29112=DIRECTION('',(0.356521352096954,0.,0.934287175069293));
#29113=DIRECTION('',(-0.715443769451104,0.,-0.69867031764173));
#29114=DIRECTION('',(-0.771525643922909,0.,-0.636198224431145));
#29115=DIRECTION('',(-0.816588132859797,0.,-0.577220773424303));
#29116=DIRECTION('',(-0.85383585346242,0.,-0.520542347309132));
#29117=DIRECTION('',(-0.885030574305658,0.,-0.465532901677419));
#29118=DIRECTION('',(-0.911263560158432,0.,-0.411823656347446));
#29119=DIRECTION('',(-0.876920914189556,0.,0.480634695228043));
#29120=DIRECTION('',(-0.869705019525388,0.,0.493571858002809));
#29121=DIRECTION('',(-0.862298277386214,0.,0.506400711706418));
#29122=DIRECTION('',(-0.854702313102447,0.,0.51911844118402));
#29123=DIRECTION('',(-0.0989820318029304,0.,0.995089220813975));
#29124=DIRECTION('',(-0.0393519680027076,0.,0.99922541131334));
#29125=DIRECTION('',(0.0238849697840824,0.,0.999714713414989));
#29126=DIRECTION('',(0.0915937869476479,0.,0.995796454197638));
#29127=DIRECTION('',(0.165201002238474,0.,0.986259919523958));
#29128=DIRECTION('',(-0.630855751991531,0.,-0.775900135442185));
#29129=DIRECTION('',(-0.742482951693498,0.,0.669864961350055));
#29130=DIRECTION('',(-0.669864961350053,0.,0.742482951693499));
#29131=DIRECTION('',(0.775900135442185,0.,0.630855751991531));
#29132=DIRECTION('',(-0.968927638144812,0.,-0.247344359222354));
#29133=DIRECTION('',(-0.986259919523961,0.,-0.165201002238458));
#29134=DIRECTION('',(-0.995796454197637,0.,-0.091593786947663));
#29135=DIRECTION('',(-0.99971471341499,0.,-0.023884969784058));
#29136=DIRECTION('',(-0.999225411313341,0.,0.0393519680026942));
#29137=DIRECTION('',(-0.995089220813975,0.,0.0989820318029307));
#29138=DIRECTION('',(-0.519118441184019,0.,0.854702313102448));
#29139=DIRECTION('',(-0.506400711706419,0.,0.862298277386214));
#29140=DIRECTION('',(-0.493571858002814,0.,0.869705019525385));
#29141=DIRECTION('',(-0.48063469522803,0.,0.876920914189563));
#29142=DIRECTION('',(0.411823656347447,0.,0.911263560158432));
#29143=DIRECTION('',(0.465532901677422,0.,0.885030574305656));
#29144=DIRECTION('',(0.520542347309115,0.,0.85383585346243));
#29145=DIRECTION('',(0.577220773424313,0.,0.81658813285979));
#29146=DIRECTION('',(0.636198224431135,0.,0.771525643922917));
#29147=DIRECTION('',(-0.934287175069293,0.,-0.356521352096954));
#29148=DIRECTION('',(-0.308076617368396,0.,0.951361549480978));
#29149=DIRECTION('',(-0.208878597787478,0.,0.977941578718451));
#29150=DIRECTION('',(0.987377104088484,0.,0.158387039627108));
#29151=DIRECTION('',(-0.962788128673439,0.,0.270257320503067));
#29152=DIRECTION('',(-0.936726646161376,0.,0.350061695092823));
#29153=DIRECTION('',(-0.908181919807451,0.,0.418575680773326));
#29154=DIRECTION('',(-0.87772082324649,0.,0.479172366105876));
#29155=DIRECTION('',(-0.845678606302961,0.,0.533692509635915));
#29156=DIRECTION('',(-0.812281528355498,0.,0.583265564466527));
#29157=DIRECTION('',(-0.0222186010871084,0.,0.99975313641205));
#29158=DIRECTION('',(-0.00740674213917776,0.,0.999972569709231));
#29159=DIRECTION('',(0.00740674213917776,0.,0.999972569709231));
#29160=DIRECTION('',(0.0222186010871084,0.,0.99975313641205));
#29161=DIRECTION('',(0.8122815283555,0.,0.583265564466524));
#29162=DIRECTION('',(0.84567860630296,0.,0.533692509635917));
#29163=DIRECTION('',(0.87772082324649,0.,0.479172366105876));
#29164=DIRECTION('',(0.908181919807451,0.,0.418575680773325));
#29165=DIRECTION('',(0.936726646161376,0.,0.350061695092823));
#29166=DIRECTION('',(-0.987377104088484,0.,0.158387039627109));
#29167=DIRECTION('',(0.20887859778748,0.,0.977941578718451));
#29168=DIRECTION('',(0.308076617368396,0.,0.951361549480978));
#29169=DIRECTION('',(0.934287175069293,0.,-0.356521352096954));
#29170=DIRECTION('',(-0.698670317641747,0.,0.715443769451087));
#29171=DIRECTION('',(-0.636198224431136,0.,0.771525643922916));
#29172=DIRECTION('',(-0.577220773424311,0.,0.816588132859791));
#29173=DIRECTION('',(-0.520542347309115,0.,0.85383585346243));
#29174=DIRECTION('',(-0.465532901677425,0.,0.885030574305655));
#29175=DIRECTION('',(-0.41182365634745,0.,0.91126356015843));
#29176=DIRECTION('',(0.480634695228042,0.,0.876920914189556));
#29177=DIRECTION('',(0.493571858002802,0.,0.869705019525391));
#29178=DIRECTION('',(0.506400711706431,0.,0.862298277386207));
#29179=DIRECTION('',(0.519118441184006,0.,0.854702313102456));
#29180=DIRECTION('',(0.995089220813975,0.,0.0989820318029304));
#29181=DIRECTION('',(0.999225411313341,0.,0.0393519680026977));
#29182=DIRECTION('',(0.99971471341499,0.,-0.0238849697840613));
#29183=DIRECTION('',(0.995796454197637,0.,-0.0915937869476627));
#29184=DIRECTION('',(0.98625991952396,0.,-0.165201002238459));
#29185=DIRECTION('',(-0.775900135442185,0.,0.63085575199153));
#29186=DIRECTION('',(0.669864961350055,0.,0.742482951693498));
#29187=DIRECTION('',(0.742482951693498,0.,0.669864961350055));
#29188=DIRECTION('',(0.63085575199153,0.,-0.775900135442185));
#29189=DIRECTION('',(-0.247344359222349,0.,0.968927638144813));
#29190=DIRECTION('',(-0.165201002238462,0.,0.98625991952396));
#29191=DIRECTION('',(-0.0915937869476591,0.,0.995796454197637));
#29192=DIRECTION('',(-0.0238849697840614,0.,0.99971471341499));
#29193=DIRECTION('',(0.0393519680026975,0.,0.999225411313341));
#29194=DIRECTION('',(0.0989820318029307,0.,0.995089220813975));
#29195=DIRECTION('',(0.85470231310245,0.,0.519118441184015));
#29196=DIRECTION('',(0.86229827738621,0.,0.506400711706427));
#29197=DIRECTION('',(0.86970501952539,0.,0.493571858002805));
#29198=DIRECTION('',(0.876920914189557,0.,0.48063469522804));
#29199=DIRECTION('',(0.911263560158429,0.,-0.411823656347453));
#29200=DIRECTION('',(0.885030574305657,0.,-0.46553290167742));
#29201=DIRECTION('',(0.853835853462428,0.,-0.520542347309119));
#29202=DIRECTION('',(0.816588132859795,0.,-0.577220773424306));
#29203=DIRECTION('',(0.771525643922911,0.,-0.636198224431142));
#29204=DIRECTION('',(-0.356521352096954,0.,0.934287175069293));
#29205=DIRECTION('',(0.951361549480978,0.,0.308076617368397));
#29206=DIRECTION('',(0.977941578718451,0.,0.208878597787479));
#29207=DIRECTION('',(0.158387039627108,0.,-0.987377104088484));
#29208=DIRECTION('',(0.270257320503068,0.,0.962788128673439));
#29209=DIRECTION('',(0.350061695092817,0.,0.936726646161378));
#29210=DIRECTION('',(0.418575680773335,0.,0.908181919807446));
#29211=DIRECTION('',(0.479172366105872,0.,0.877720823246493));
#29212=DIRECTION('',(0.533692509635919,0.,0.845678606302959));
#29213=DIRECTION('',(0.583265564466523,0.,0.812281528355501));
#29214=DIRECTION('',(0.99975313641205,0.,0.0222186010871085));
#29215=DIRECTION('',(0.999972569709231,0.,0.00740674213917776));
#29216=DIRECTION('',(0.999972569709231,0.,-0.00740674213917776));
#29217=DIRECTION('',(0.99975313641205,0.,-0.0222186010871084));
#29218=DIRECTION('',(0.583265564466523,0.,-0.812281528355501));
#29219=DIRECTION('',(0.533692509635919,0.,-0.845678606302959));
#29220=DIRECTION('',(0.479172366105872,0.,-0.877720823246493));
#29221=DIRECTION('',(0.418575680773335,0.,-0.908181919807446));
#29222=DIRECTION('',(0.350061695092817,0.,-0.936726646161378));
#29223=DIRECTION('',(0.158387039627108,0.,0.987377104088484));
#29224=DIRECTION('',(0.977941578718451,0.,-0.208878597787478));
#29225=DIRECTION('',(0.951361549480978,0.,-0.308076617368396));
#29226=DIRECTION('',(-0.356521352096954,0.,-0.934287175069293));
#29227=DIRECTION('',(0.715443769451087,0.,0.698670317641747));
#29228=DIRECTION('',(0.771525643922913,0.,0.63619822443114));
#29229=DIRECTION('',(0.816588132859796,0.,0.577220773424304));
#29230=DIRECTION('',(0.853835853462428,0.,0.520542347309119));
#29231=DIRECTION('',(0.885030574305657,0.,0.465532901677421));
#29232=DIRECTION('',(0.911263560158431,0.,0.411823656347449));
#29233=DIRECTION('',(0.876920914189562,0.,-0.480634695228032));
#29234=DIRECTION('',(0.869705019525386,0.,-0.493571858002812));
#29235=DIRECTION('',(0.862298277386212,0.,-0.506400711706423));
#29236=DIRECTION('',(0.85470231310245,0.,-0.519118441184015));
#29237=DIRECTION('',(0.0989820318029246,0.,-0.995089220813975));
#29238=DIRECTION('',(0.0393519680027008,0.,-0.999225411313341));
#29239=DIRECTION('',(-0.0238849697840649,0.,-0.999714713414989));
#29240=DIRECTION('',(-0.0915937869476482,0.,-0.995796454197638));
#29241=DIRECTION('',(-0.165201002238466,0.,-0.986259919523959));
#29242=DIRECTION('',(0.63085575199153,0.,0.775900135442185));
#29243=DIRECTION('',(0.742482951693498,0.,-0.669864961350055));
#29244=DIRECTION('',(0.669864961350055,0.,-0.742482951693498));
#29245=DIRECTION('',(-0.775900135442185,0.,-0.63085575199153));
#29246=DIRECTION('',(0.968927638144813,0.,0.247344359222349));
#29247=DIRECTION('',(0.986259919523959,0.,0.165201002238466));
#29248=DIRECTION('',(0.995796454197638,0.,0.0915937869476553));
#29249=DIRECTION('',(0.999714713414989,0.,0.0238849697840649));
#29250=DIRECTION('',(0.99922541131334,0.,-0.039351968002701));
#29251=DIRECTION('',(0.995089220813975,0.,-0.0989820318029272));
#29252=DIRECTION('',(0.519118441184011,0.,-0.854702313102452));
#29253=DIRECTION('',(0.506400711706425,0.,-0.862298277386211));
#29254=DIRECTION('',(0.493571858002802,0.,-0.869705019525391));
#29255=DIRECTION('',(0.480634695228039,0.,-0.876920914189558));
#29256=DIRECTION('',(-0.411823656347455,0.,-0.911263560158428));
#29257=DIRECTION('',(-0.465532901677421,0.,-0.885030574305657));
#29258=DIRECTION('',(-0.520542347309117,0.,-0.853835853462429));
#29259=DIRECTION('',(-0.577220773424305,0.,-0.816588132859795));
#29260=DIRECTION('',(-0.636198224431141,0.,-0.771525643922912));
#29261=DIRECTION('',(0.934287175069293,0.,0.356521352096954));
#29262=DIRECTION('',(0.308076617368396,0.,-0.951361549480978));
#29263=DIRECTION('',(0.208878597787478,0.,-0.977941578718451));
#29264=DIRECTION('',(-0.987377104088484,0.,-0.158387039627108));
#29265=DIRECTION('',(0.962788128673439,0.,-0.270257320503068));
#29266=DIRECTION('',(0.936726646161378,0.,-0.350061695092817));
#29267=DIRECTION('',(0.908181919807447,0.,-0.418575680773333));
#29268=DIRECTION('',(0.877720823246493,0.,-0.479172366105871));
#29269=DIRECTION('',(0.845678606302959,0.,-0.533692509635919));
#29270=DIRECTION('',(0.812281528355501,0.,-0.583265564466523));
#29271=DIRECTION('',(0.0222186010871084,0.,-0.99975313641205));
#29272=DIRECTION('',(0.00740674213917775,0.,-0.999972569709231));
#29273=DIRECTION('',(-0.00740674213917775,0.,-0.999972569709231));
#29274=DIRECTION('',(-0.0222186010871084,0.,-0.99975313641205));
#29275=DIRECTION('',(-0.812281528355501,0.,-0.583265564466523));
#29276=DIRECTION('',(-0.845678606302959,0.,-0.533692509635919));
#29277=DIRECTION('',(-0.877720823246493,0.,-0.479172366105871));
#29278=DIRECTION('',(-0.908181919807447,0.,-0.418575680773333));
#29279=DIRECTION('',(-0.936726646161378,0.,-0.350061695092817));
#29280=DIRECTION('',(0.987377104088484,0.,-0.158387039627108));
#29281=DIRECTION('',(-0.208878597787478,0.,-0.977941578718451));
#29282=DIRECTION('',(-0.308076617368396,0.,-0.951361549480978));
#29283=DIRECTION('',(-0.934287175069293,0.,0.356521352096954));
#29284=DIRECTION('',(0.698670317641746,0.,-0.715443769451088));
#29285=DIRECTION('',(0.636198224431141,0.,-0.771525643922912));
#29286=DIRECTION('',(0.577220773424305,0.,-0.816588132859795));
#29287=DIRECTION('',(0.520542347309117,0.,-0.853835853462429));
#29288=DIRECTION('',(0.465532901677421,0.,-0.885030574305657));
#29289=DIRECTION('',(0.411823656347455,0.,-0.911263560158428));
#29290=DIRECTION('',(-0.480634695228039,0.,-0.876920914189558));
#29291=DIRECTION('',(-0.493571858002802,0.,-0.869705019525391));
#29292=DIRECTION('',(-0.506400711706425,0.,-0.862298277386211));
#29293=DIRECTION('',(-0.519118441184011,0.,-0.854702313102452));
#29294=DIRECTION('',(-0.995089220813975,0.,-0.0989820318029272));
#29295=DIRECTION('',(-0.99922541131334,0.,-0.039351968002701));
#29296=DIRECTION('',(-0.999714713414989,0.,0.0238849697840649));
#29297=DIRECTION('',(-0.995796454197638,0.,0.0915937869476553));
#29298=DIRECTION('',(-0.986259919523959,0.,0.165201002238466));
#29299=DIRECTION('',(0.775900135442185,0.,-0.63085575199153));
#29300=DIRECTION('',(-0.669864961350055,0.,-0.742482951693498));
#29301=DIRECTION('',(-0.742482951693498,0.,-0.669864961350055));
#29302=DIRECTION('',(-0.63085575199153,0.,0.775900135442185));
#29303=DIRECTION('',(0.247344359222354,0.,-0.968927638144812));
#29304=DIRECTION('',(0.165201002238466,0.,-0.986259919523959));
#29305=DIRECTION('',(0.0915937869476482,0.,-0.995796454197638));
#29306=DIRECTION('',(0.0238849697840649,0.,-0.999714713414989));
#29307=DIRECTION('',(-0.0393519680027008,0.,-0.999225411313341));
#29308=DIRECTION('',(-0.0989820318029246,0.,-0.995089220813975));
#29309=DIRECTION('',(-0.85470231310245,0.,-0.519118441184015));
#29310=DIRECTION('',(-0.862298277386212,0.,-0.506400711706423));
#29311=DIRECTION('',(-0.869705019525386,0.,-0.493571858002812));
#29312=DIRECTION('',(-0.876920914189562,0.,-0.480634695228032));
#29313=DIRECTION('',(-0.911263560158431,0.,0.411823656347449));
#29314=DIRECTION('',(-0.885030574305657,0.,0.465532901677421));
#29315=DIRECTION('',(-0.853835853462428,0.,0.520542347309119));
#29316=DIRECTION('',(-0.816588132859796,0.,0.577220773424304));
#29317=DIRECTION('',(-0.771525643922913,0.,0.63619822443114));
#29318=DIRECTION('',(0.356521352096954,0.,-0.934287175069293));
#29319=DIRECTION('',(-0.951361549480978,0.,-0.308076617368396));
#29320=DIRECTION('',(-0.977941578718451,0.,-0.208878597787478));
#29321=DIRECTION('',(-0.158387039627108,0.,0.987377104088484));
#29322=DIRECTION('',(-0.270257320503068,0.,-0.962788128673439));
#29323=DIRECTION('',(-0.350061695092817,0.,-0.936726646161378));
#29324=DIRECTION('',(-0.418575680773335,0.,-0.908181919807446));
#29325=DIRECTION('',(-0.479172366105872,0.,-0.877720823246493));
#29326=DIRECTION('',(-0.533692509635919,0.,-0.845678606302959));
#29327=DIRECTION('',(-0.583265564466523,0.,-0.812281528355501));
#29328=DIRECTION('',(-0.99975313641205,0.,-0.0222186010871084));
#29329=DIRECTION('',(-0.999972569709231,0.,-0.00740674213917776));
#29330=DIRECTION('',(-0.999972569709231,0.,0.00740674213917776));
#29331=DIRECTION('',(-0.99975313641205,0.,0.0222186010871085));
#29332=DIRECTION('',(-0.583265564466523,0.,0.812281528355501));
#29333=DIRECTION('',(-0.533692509635919,0.,0.845678606302959));
#29334=DIRECTION('',(-0.479172366105872,0.,0.877720823246493));
#29335=DIRECTION('',(-0.418575680773335,0.,0.908181919807446));
#29336=DIRECTION('',(-0.350061695092817,0.,0.936726646161378));
#29337=DIRECTION('center_axis',(0.,1.,0.));
#29338=DIRECTION('ref_axis',(0.,0.,1.));
#29339=DIRECTION('center_axis',(0.698181045889302,0.707106781186549,0.11199654977239));
#29340=DIRECTION('ref_axis',(0.158387039627108,0.,-0.987377104088484));
#29341=DIRECTION('',(-0.249231185799881,0.386714295024741,-0.887882801977999));
#29342=DIRECTION('',(-0.69196539626054,0.706639907076675,-0.147796928603616));
#29343=DIRECTION('',(-0.163114865717534,0.309436927624311,-0.936825665961591));
#29344=DIRECTION('center_axis',(-0.660640797067119,0.707106781186548,-0.252098665705553));
#29345=DIRECTION('ref_axis',(-0.356521352096954,0.,0.934287175069293));
#29346=DIRECTION('',(-0.510131065430303,-0.176491388068496,0.841793968866848));
#29347=DIRECTION('',(-0.356521352096954,0.,0.934287175069293));
#29348=DIRECTION('',(-0.673158076003201,-0.706639907076675,-0.217986803358222));
#29349=DIRECTION('center_axis',(0.548644247294729,0.707106781186549,0.446082380183749));
#29350=DIRECTION('ref_axis',(0.63085575199153,0.,-0.775900135442185));
#29351=DIRECTION('',(0.228100862670987,0.386714295024739,-0.893544654996196));
#29352=DIRECTION('',(-0.525361147399584,0.706639907076675,-0.473978592902317));
#29353=DIRECTION('',(0.327151215534519,0.309436927624314,-0.89287225849878));
#29354=DIRECTION('center_axis',(-0.446082380183748,0.707106781186549,-0.548644247294729));
#29355=DIRECTION('ref_axis',(-0.775900135442186,0.,0.63085575199153));
#29356=DIRECTION('',(-0.862683446355689,-0.176491388068498,0.473949429076063));
#29357=DIRECTION('',(-0.775900135442185,0.,0.63085575199153));
#29358=DIRECTION('',(-0.473978592902317,-0.706639907076675,-0.525361147399585));
#29359=DIRECTION('center_axis',(0.252098665705552,0.707106781186548,0.66064079706712));
#29360=DIRECTION('ref_axis',(0.934287175069293,0.,-0.356521352096954));
#29361=DIRECTION('',(0.644313469196316,0.386714295024741,-0.659781939307015));
#29362=DIRECTION('',(-0.217986803358223,0.706639907076676,-0.673158076003201));
#29363=DIRECTION('',(0.729757392781242,0.309436927624314,-0.609674450427069));
#29364=DIRECTION('center_axis',(-0.11199654977239,0.707106781186549,-0.698181045889302));
#29365=DIRECTION('ref_axis',(-0.987377104088484,0.,0.158387039627108));
#29366=DIRECTION('',(-0.984080494506367,-0.176491388068501,-0.0208894774888451));
#29367=DIRECTION('',(-0.987377104088484,0.,0.158387039627108));
#29368=DIRECTION('',(-0.147796928603616,-0.706639907076675,-0.691965396260539));
#29369=DIRECTION('center_axis',(-0.11199654977239,0.707106781186549,0.698181045889302));
#29370=DIRECTION('ref_axis',(0.987377104088484,0.,0.158387039627108));
#29371=DIRECTION('',(0.887882801977998,0.386714295024742,-0.249231185799882));
#29372=DIRECTION('',(0.147796928603616,0.706639907076675,-0.69196539626054));
#29373=DIRECTION('',(0.936825665961591,0.309436927624309,-0.163114865717533));
#29374=DIRECTION('center_axis',(0.252098665705552,0.707106781186548,-0.660640797067119));
#29375=DIRECTION('ref_axis',(-0.934287175069293,0.,-0.356521352096954));
#29376=DIRECTION('',(-0.841793968866845,-0.1764913880685,-0.510131065430306));
#29377=DIRECTION('',(-0.934287175069293,0.,-0.356521352096954));
#29378=DIRECTION('',(0.217986803358223,-0.706639907076675,-0.673158076003201));
#29379=DIRECTION('center_axis',(-0.446082380183749,0.707106781186548,0.54864424729473));
#29380=DIRECTION('ref_axis',(0.775900135442186,0.,0.63085575199153));
#29381=DIRECTION('',(0.893544654996196,0.386714295024742,0.228100862670982));
#29382=DIRECTION('',(0.473978592902316,0.706639907076676,-0.525361147399584));
#29383=DIRECTION('',(0.89287225849878,0.30943692762431,0.327151215534523));
#29384=DIRECTION('center_axis',(0.548644247294728,0.70710678118655,-0.446082380183749));
#29385=DIRECTION('ref_axis',(-0.63085575199153,0.,-0.775900135442185));
#29386=DIRECTION('',(-0.473949429076065,-0.176491388068497,-0.862683446355688));
#29387=DIRECTION('',(-0.63085575199153,0.,-0.775900135442185));
#29388=DIRECTION('',(0.525361147399585,-0.706639907076674,-0.473978592902318));
#29389=DIRECTION('center_axis',(-0.66064079706712,0.707106781186548,0.252098665705553));
#29390=DIRECTION('ref_axis',(0.356521352096954,0.,0.934287175069293));
#29391=DIRECTION('',(0.659781939307015,0.38671429502474,0.644313469196317));
#29392=DIRECTION('',(0.673158076003201,0.706639907076676,-0.217986803358222));
#29393=DIRECTION('',(0.60967445042707,0.309436927624314,0.729757392781241));
#29394=DIRECTION('center_axis',(0.698181045889302,0.707106781186549,-0.11199654977239));
#29395=DIRECTION('ref_axis',(-0.158387039627108,0.,-0.987377104088484));
#29396=DIRECTION('',(0.0208894774888416,-0.176491388068498,-0.984080494506368));
#29397=DIRECTION('',(-0.158387039627108,0.,-0.987377104088484));
#29398=DIRECTION('',(0.691965396260539,-0.706639907076675,-0.147796928603616));
#29399=DIRECTION('center_axis',(-0.698181045889302,0.707106781186549,-0.111996549772391));
#29400=DIRECTION('ref_axis',(-0.158387039627108,0.,0.987377104088484));
#29401=DIRECTION('',(0.249231185799882,0.386714295024742,0.887882801977999));
#29402=DIRECTION('',(0.691965396260539,0.706639907076675,0.147796928603617));
#29403=DIRECTION('',(0.163114865717534,0.309436927624311,0.936825665961591));
#29404=DIRECTION('center_axis',(0.660640797067119,0.707106781186549,0.252098665705552));
#29405=DIRECTION('ref_axis',(0.356521352096954,0.,-0.934287175069293));
#29406=DIRECTION('',(0.510131065430304,-0.176491388068498,-0.841793968866847));
#29407=DIRECTION('',(0.356521352096954,0.,-0.934287175069293));
#29408=DIRECTION('',(0.673158076003201,-0.706639907076675,0.217986803358224));
#29409=DIRECTION('center_axis',(-0.54864424729473,0.707106781186548,-0.446082380183749));
#29410=DIRECTION('ref_axis',(-0.63085575199153,0.,0.775900135442186));
#29411=DIRECTION('',(-0.228100862670983,0.386714295024742,0.893544654996196));
#29412=DIRECTION('',(0.525361147399584,0.706639907076676,0.473978592902316));
#29413=DIRECTION('',(-0.327151215534528,0.309436927624306,0.892872258498779));
#29414=DIRECTION('center_axis',(0.446082380183749,0.70710678118655,0.548644247294728));
#29415=DIRECTION('ref_axis',(0.775900135442185,0.,-0.63085575199153));
#29416=DIRECTION('',(0.862683446355692,-0.176491388068509,-0.473949429076052));
#29417=DIRECTION('',(0.775900135442185,0.,-0.63085575199153));
#29418=DIRECTION('',(0.473978592902318,-0.706639907076674,0.525361147399585));
#29419=DIRECTION('center_axis',(-0.252098665705553,0.707106781186548,-0.66064079706712));
#29420=DIRECTION('ref_axis',(-0.934287175069293,0.,0.356521352096954));
#29421=DIRECTION('',(-0.644313469196317,0.38671429502474,0.659781939307015));
#29422=DIRECTION('',(0.217986803358222,0.706639907076676,0.6731580760032));
#29423=DIRECTION('',(-0.729757392781247,0.309436927624309,0.609674450427066));
#29424=DIRECTION('center_axis',(0.111996549772391,0.707106781186548,0.698181045889302));
#29425=DIRECTION('ref_axis',(0.987377104088484,0.,-0.158387039627109));
#29426=DIRECTION('',(0.984080494506366,-0.176491388068509,0.0208894774888531));
#29427=DIRECTION('',(0.987377104088484,0.,-0.158387039627109));
#29428=DIRECTION('',(0.147796928603617,-0.706639907076676,0.691965396260539));
#29429=DIRECTION('center_axis',(0.11199654977239,0.707106781186549,-0.698181045889302));
#29430=DIRECTION('ref_axis',(-0.987377104088484,0.,-0.158387039627108));
#29431=DIRECTION('',(-0.887882801977999,0.386714295024741,0.249231185799881));
#29432=DIRECTION('',(-0.147796928603616,0.706639907076675,0.691965396260539));
#29433=DIRECTION('',(-0.936825665961593,0.309436927624307,0.16311486571753));
#29434=DIRECTION('center_axis',(-0.252098665705552,0.707106781186548,0.660640797067119));
#29435=DIRECTION('ref_axis',(0.934287175069293,0.,0.356521352096954));
#29436=DIRECTION('',(0.841793968866839,-0.176491388068509,0.510131065430313));
#29437=DIRECTION('',(0.934287175069293,0.,0.356521352096954));
#29438=DIRECTION('',(-0.217986803358223,-0.706639907076675,0.673158076003201));
#29439=DIRECTION('center_axis',(0.446082380183749,0.70710678118655,-0.548644247294728));
#29440=DIRECTION('ref_axis',(-0.775900135442185,0.,-0.630855751991531));
#29441=DIRECTION('',(-0.893544654996196,0.386714295024738,-0.228100862670987));
#29442=DIRECTION('',(-0.473978592902316,0.706639907076674,0.525361147399586));
#29443=DIRECTION('',(-0.892872258498779,0.309436927624308,-0.327151215534526));
#29444=DIRECTION('center_axis',(-0.548644247294728,0.70710678118655,0.446082380183749));
#29445=DIRECTION('ref_axis',(0.630855751991531,0.,0.775900135442185));
#29446=DIRECTION('',(0.473949429076065,-0.176491388068498,0.862683446355688));
#29447=DIRECTION('',(0.630855751991531,0.,0.775900135442185));
#29448=DIRECTION('',(-0.525361147399585,-0.706639907076674,0.473978592902317));
#29449=DIRECTION('center_axis',(0.660640797067119,0.707106781186549,-0.252098665705553));
#29450=DIRECTION('ref_axis',(-0.356521352096954,0.,-0.934287175069293));
#29451=DIRECTION('',(-0.659781939307025,0.386714295024756,-0.644313469196296));
#29452=DIRECTION('',(-0.673158076003201,0.706639907076675,0.217986803358222));
#29453=DIRECTION('',(-0.609674450427067,0.309436927624308,-0.729757392781247));
#29454=DIRECTION('center_axis',(0.,-1.,0.));
#29455=DIRECTION('ref_axis',(-1.,0.,0.));
#29456=DIRECTION('center_axis',(0.,-1.,0.));
#29457=DIRECTION('ref_axis',(0.,0.,1.));
#29458=DIRECTION('',(0.,0.,-1.));
#29459=DIRECTION('',(-1.,0.,0.));
#29460=DIRECTION('',(0.,0.,-1.));
#29461=DIRECTION('center_axis',(-1.,0.,0.));
#29462=DIRECTION('ref_axis',(0.,1.,0.));
#29463=DIRECTION('',(0.,1.,0.));
#29464=DIRECTION('',(0.,1.,0.));
#29465=DIRECTION('',(0.,0.,-1.));
#29466=DIRECTION('center_axis',(1.,0.,0.));
#29467=DIRECTION('ref_axis',(0.,-1.,0.));
#29468=DIRECTION('',(0.,-1.,0.));
#29469=DIRECTION('',(0.,0.,-1.));
#29470=DIRECTION('',(0.,-1.,0.));
#29471=DIRECTION('center_axis',(0.,1.,0.));
#29472=DIRECTION('ref_axis',(1.,0.,0.));
#29473=DIRECTION('center_axis',(0.,1.,0.));
#29474=DIRECTION('ref_axis',(0.,0.,1.));
#29475=DIRECTION('',(1.,0.,0.));
#29476=DIRECTION('center_axis',(0.,0.,-1.));
#29477=DIRECTION('ref_axis',(-1.,0.,0.));
#29478=DIRECTION('center_axis',(-0.20887859778748,0.,-0.977941578718451));
#29479=DIRECTION('ref_axis',(-0.977941578718451,0.,0.20887859778748));
#29480=DIRECTION('',(0.,1.,0.));
#29481=DIRECTION('',(0.,1.,0.));
#29482=DIRECTION('center_axis',(-0.987377104088484,0.,0.158387039627108));
#29483=DIRECTION('ref_axis',(0.158387039627108,0.,0.987377104088484));
#29484=DIRECTION('',(0.,1.,0.));
#29485=DIRECTION('center_axis',(-0.999774774701824,0.,-0.0212226263670861));
#29486=DIRECTION('ref_axis',(-0.0212226263670861,0.,0.999774774701824));
#29487=DIRECTION('center_axis',(-0.936726646161378,0.,-0.350061695092817));
#29488=DIRECTION('ref_axis',(-0.350061695092817,0.,0.936726646161378));
#29489=DIRECTION('',(0.,1.,0.));
#29490=DIRECTION('center_axis',(-0.908181919807446,0.,-0.418575680773336));
#29491=DIRECTION('ref_axis',(-0.418575680773336,0.,0.908181919807446));
#29492=DIRECTION('',(0.,1.,0.));
#29493=DIRECTION('center_axis',(-0.877720823246492,0.,-0.479172366105872));
#29494=DIRECTION('ref_axis',(-0.479172366105872,0.,0.877720823246493));
#29495=DIRECTION('',(0.,1.,0.));
#29496=DIRECTION('center_axis',(-0.845678606302959,0.,-0.533692509635919));
#29497=DIRECTION('ref_axis',(-0.533692509635919,0.,0.845678606302959));
#29498=DIRECTION('',(0.,1.,0.));
#29499=DIRECTION('center_axis',(-0.812281528355501,0.,-0.583265564466523));
#29500=DIRECTION('ref_axis',(-0.583265564466523,0.,0.812281528355501));
#29501=DIRECTION('',(0.,1.,0.));
#29502=DIRECTION('center_axis',(-0.0222186010871085,0.,-0.999753136412051));
#29503=DIRECTION('ref_axis',(-0.99975313641205,0.,0.0222186010871085));
#29504=DIRECTION('',(0.,1.,0.));
#29505=DIRECTION('center_axis',(-0.00740674213917776,0.,-0.999972569709231));
#29506=DIRECTION('ref_axis',(-0.999972569709231,0.,0.00740674213917776));
#29507=DIRECTION('',(0.,1.,0.));
#29508=DIRECTION('center_axis',(0.00740674213917776,0.,-0.999972569709231));
#29509=DIRECTION('ref_axis',(-0.999972569709231,0.,-0.00740674213917776));
#29510=DIRECTION('',(0.,1.,0.));
#29511=DIRECTION('center_axis',(0.0222186010871084,0.,-0.999753136412051));
#29512=DIRECTION('ref_axis',(-0.99975313641205,0.,-0.0222186010871084));
#29513=DIRECTION('',(0.,1.,0.));
#29514=DIRECTION('center_axis',(0.812281528355501,0.,-0.583265564466523));
#29515=DIRECTION('ref_axis',(-0.583265564466523,0.,-0.812281528355501));
#29516=DIRECTION('',(0.,1.,0.));
#29517=DIRECTION('center_axis',(0.845678606302959,0.,-0.533692509635919));
#29518=DIRECTION('ref_axis',(-0.533692509635919,0.,-0.845678606302959));
#29519=DIRECTION('',(0.,1.,0.));
#29520=DIRECTION('center_axis',(0.877720823246492,0.,-0.479172366105872));
#29521=DIRECTION('ref_axis',(-0.479172366105872,0.,-0.877720823246493));
#29522=DIRECTION('',(0.,1.,0.));
#29523=DIRECTION('center_axis',(0.908181919807446,0.,-0.418575680773335));
#29524=DIRECTION('ref_axis',(-0.418575680773335,0.,-0.908181919807446));
#29525=DIRECTION('',(0.,1.,0.));
#29526=DIRECTION('center_axis',(0.936726646161378,0.,-0.350061695092817));
#29527=DIRECTION('ref_axis',(-0.350061695092817,0.,-0.936726646161378));
#29528=DIRECTION('',(0.,1.,0.));
#29529=DIRECTION('center_axis',(0.962788128673439,0.,-0.270257320503068));
#29530=DIRECTION('ref_axis',(-0.270257320503068,0.,-0.962788128673439));
#29531=DIRECTION('',(0.,1.,0.));
#29532=DIRECTION('center_axis',(0.985178244547962,0.,-0.171533747319286));
#29533=DIRECTION('ref_axis',(-0.171533747319286,0.,-0.985178244547962));
#29534=DIRECTION('center_axis',(0.208878597787478,0.,-0.977941578718451));
#29535=DIRECTION('ref_axis',(-0.977941578718451,0.,-0.208878597787478));
#29536=DIRECTION('',(0.,1.,0.));
#29537=DIRECTION('center_axis',(0.308076617368396,0.,-0.951361549480978));
#29538=DIRECTION('ref_axis',(-0.951361549480978,0.,-0.308076617368396));
#29539=DIRECTION('',(0.,1.,0.));
#29540=DIRECTION('center_axis',(-0.934287175069293,0.,-0.356521352096954));
#29541=DIRECTION('ref_axis',(-0.356521352096954,0.,0.934287175069293));
#29542=DIRECTION('',(0.,1.,0.));
#29543=DIRECTION('center_axis',(-0.855219039771101,0.,-0.518266720919832));
#29544=DIRECTION('ref_axis',(-0.518266720919832,0.,0.855219039771102));
#29545=DIRECTION('center_axis',(-0.63619822443114,0.,-0.771525643922913));
#29546=DIRECTION('ref_axis',(-0.771525643922913,0.,0.63619822443114));
#29547=DIRECTION('',(0.,1.,0.));
#29548=DIRECTION('center_axis',(-0.577220773424304,0.,-0.816588132859796));
#29549=DIRECTION('ref_axis',(-0.816588132859796,0.,0.577220773424304));
#29550=DIRECTION('',(0.,1.,0.));
#29551=DIRECTION('center_axis',(-0.520542347309119,0.,-0.853835853462428));
#29552=DIRECTION('ref_axis',(-0.853835853462428,0.,0.520542347309119));
#29553=DIRECTION('',(0.,1.,0.));
#29554=DIRECTION('center_axis',(-0.465532901677421,0.,-0.885030574305657));
#29555=DIRECTION('ref_axis',(-0.885030574305657,0.,0.465532901677421));
#29556=DIRECTION('',(0.,1.,0.));
#29557=DIRECTION('center_axis',(-0.411823656347449,0.,-0.911263560158431));
#29558=DIRECTION('ref_axis',(-0.911263560158431,0.,0.411823656347449));
#29559=DIRECTION('',(0.,1.,0.));
#29560=DIRECTION('center_axis',(0.480634695228032,0.,-0.876920914189562));
#29561=DIRECTION('ref_axis',(-0.876920914189562,0.,-0.480634695228032));
#29562=DIRECTION('',(0.,1.,0.));
#29563=DIRECTION('center_axis',(0.493571858002813,0.,-0.869705019525386));
#29564=DIRECTION('ref_axis',(-0.869705019525386,0.,-0.493571858002812));
#29565=DIRECTION('',(0.,1.,0.));
#29566=DIRECTION('center_axis',(0.506400711706423,0.,-0.862298277386212));
#29567=DIRECTION('ref_axis',(-0.862298277386212,0.,-0.506400711706423));
#29568=DIRECTION('',(0.,1.,0.));
#29569=DIRECTION('center_axis',(0.519118441184015,0.,-0.85470231310245));
#29570=DIRECTION('ref_axis',(-0.85470231310245,0.,-0.519118441184015));
#29571=DIRECTION('',(0.,1.,0.));
#29572=DIRECTION('center_axis',(0.995089220813976,0.,-0.0989820318029246));
#29573=DIRECTION('ref_axis',(-0.0989820318029246,0.,-0.995089220813976));
#29574=DIRECTION('',(0.,1.,0.));
#29575=DIRECTION('center_axis',(0.999225411313341,0.,-0.0393519680027008));
#29576=DIRECTION('ref_axis',(-0.0393519680027008,0.,-0.999225411313341));
#29577=DIRECTION('',(0.,1.,0.));
#29578=DIRECTION('center_axis',(0.999714713414989,0.,0.0238849697840649));
#29579=DIRECTION('ref_axis',(0.0238849697840649,0.,-0.99971471341499));
#29580=DIRECTION('',(0.,1.,0.));
#29581=DIRECTION('center_axis',(0.995796454197638,0.,0.0915937869476482));
#29582=DIRECTION('ref_axis',(0.0915937869476482,0.,-0.995796454197638));
#29583=DIRECTION('',(0.,1.,0.));
#29584=DIRECTION('center_axis',(0.986259919523959,0.,0.165201002238466));
#29585=DIRECTION('ref_axis',(0.165201002238466,0.,-0.986259919523959));
#29586=DIRECTION('',(0.,1.,0.));
#29587=DIRECTION('center_axis',(0.968927638144812,0.,0.247344359222354));
#29588=DIRECTION('ref_axis',(0.247344359222354,0.,-0.968927638144812));
#29589=DIRECTION('',(0.,1.,0.));
#29590=DIRECTION('center_axis',(0.938956260693937,0.,0.344036539489135));
#29591=DIRECTION('ref_axis',(0.344036539489135,0.,-0.938956260693937));
#29592=DIRECTION('center_axis',(0.669864961350055,0.,-0.742482951693498));
#29593=DIRECTION('ref_axis',(-0.742482951693498,0.,-0.669864961350055));
#29594=DIRECTION('',(0.,1.,0.));
#29595=DIRECTION('center_axis',(0.742482951693498,0.,-0.669864961350055));
#29596=DIRECTION('ref_axis',(-0.669864961350055,0.,-0.742482951693498));
#29597=DIRECTION('',(0.,1.,0.));
#29598=DIRECTION('center_axis',(-0.63085575199153,0.,-0.775900135442186));
#29599=DIRECTION('ref_axis',(-0.775900135442185,0.,0.63085575199153));
#29600=DIRECTION('',(0.,1.,0.));
#29601=DIRECTION('center_axis',(-0.481508053781989,0.,-0.876441666138187));
#29602=DIRECTION('ref_axis',(-0.876441666138187,0.,0.481508053781989));
#29603=DIRECTION('center_axis',(-0.165201002238466,0.,-0.986259919523959));
#29604=DIRECTION('ref_axis',(-0.986259919523959,0.,0.165201002238466));
#29605=DIRECTION('',(0.,1.,0.));
#29606=DIRECTION('center_axis',(-0.0915937869476553,0.,-0.995796454197638));
#29607=DIRECTION('ref_axis',(-0.995796454197638,0.,0.0915937869476553));
#29608=DIRECTION('',(0.,1.,0.));
#29609=DIRECTION('center_axis',(-0.0238849697840649,0.,-0.999714713414989));
#29610=DIRECTION('ref_axis',(-0.99971471341499,0.,0.0238849697840649));
#29611=DIRECTION('',(0.,1.,0.));
#29612=DIRECTION('center_axis',(0.039351968002701,0.,-0.999225411313341));
#29613=DIRECTION('ref_axis',(-0.99922541131334,0.,-0.039351968002701));
#29614=DIRECTION('',(0.,1.,0.));
#29615=DIRECTION('center_axis',(0.0989820318029272,0.,-0.995089220813975));
#29616=DIRECTION('ref_axis',(-0.995089220813975,0.,-0.0989820318029272));
#29617=DIRECTION('',(0.,1.,0.));
#29618=DIRECTION('center_axis',(0.854702313102452,0.,-0.519118441184011));
#29619=DIRECTION('ref_axis',(-0.519118441184011,0.,-0.854702313102452));
#29620=DIRECTION('',(0.,1.,0.));
#29621=DIRECTION('center_axis',(0.862298277386211,0.,-0.506400711706425));
#29622=DIRECTION('ref_axis',(-0.506400711706425,0.,-0.862298277386211));
#29623=DIRECTION('',(0.,1.,0.));
#29624=DIRECTION('center_axis',(0.869705019525391,0.,-0.493571858002802));
#29625=DIRECTION('ref_axis',(-0.493571858002802,0.,-0.869705019525391));
#29626=DIRECTION('',(0.,1.,0.));
#29627=DIRECTION('center_axis',(0.876920914189558,0.,-0.480634695228039));
#29628=DIRECTION('ref_axis',(-0.480634695228039,0.,-0.876920914189558));
#29629=DIRECTION('',(0.,1.,0.));
#29630=DIRECTION('center_axis',(0.911263560158428,0.,0.411823656347455));
#29631=DIRECTION('ref_axis',(0.411823656347455,0.,-0.911263560158428));
#29632=DIRECTION('',(0.,1.,0.));
#29633=DIRECTION('center_axis',(0.885030574305657,0.,0.465532901677421));
#29634=DIRECTION('ref_axis',(0.465532901677421,0.,-0.885030574305657));
#29635=DIRECTION('',(0.,1.,0.));
#29636=DIRECTION('center_axis',(0.853835853462429,0.,0.520542347309117));
#29637=DIRECTION('ref_axis',(0.520542347309117,0.,-0.853835853462429));
#29638=DIRECTION('',(0.,1.,0.));
#29639=DIRECTION('center_axis',(0.816588132859795,0.,0.577220773424305));
#29640=DIRECTION('ref_axis',(0.577220773424305,0.,-0.816588132859795));
#29641=DIRECTION('',(0.,1.,0.));
#29642=DIRECTION('center_axis',(0.771525643922912,0.,0.636198224431141));
#29643=DIRECTION('ref_axis',(0.636198224431141,0.,-0.771525643922912));
#29644=DIRECTION('',(0.,1.,0.));
#29645=DIRECTION('center_axis',(0.715443769451088,0.,0.698670317641746));
#29646=DIRECTION('ref_axis',(0.698670317641746,0.,-0.715443769451088));
#29647=DIRECTION('',(0.,1.,0.));
#29648=DIRECTION('center_axis',(0.641141705058826,0.,0.767422513374648));
#29649=DIRECTION('ref_axis',(0.767422513374648,0.,-0.641141705058826));
#29650=DIRECTION('center_axis',(0.951361549480978,0.,-0.308076617368396));
#29651=DIRECTION('ref_axis',(-0.308076617368396,0.,-0.951361549480978));
#29652=DIRECTION('',(0.,1.,0.));
#29653=DIRECTION('center_axis',(0.977941578718451,0.,-0.208878597787478));
#29654=DIRECTION('ref_axis',(-0.208878597787478,0.,-0.977941578718451));
#29655=DIRECTION('',(0.,1.,0.));
#29656=DIRECTION('center_axis',(-0.158387039627108,0.,-0.987377104088484));
#29657=DIRECTION('ref_axis',(-0.987377104088484,0.,0.158387039627108));
#29658=DIRECTION('',(0.,1.,0.));
#29659=DIRECTION('center_axis',(0.0212226263670891,0.,-0.999774774701824));
#29660=DIRECTION('ref_axis',(-0.999774774701824,0.,-0.0212226263670891));
#29661=DIRECTION('center_axis',(0.350061695092817,0.,-0.936726646161378));
#29662=DIRECTION('ref_axis',(-0.936726646161378,0.,-0.350061695092817));
#29663=DIRECTION('',(0.,1.,0.));
#29664=DIRECTION('center_axis',(0.418575680773333,0.,-0.908181919807447));
#29665=DIRECTION('ref_axis',(-0.908181919807447,0.,-0.418575680773333));
#29666=DIRECTION('',(0.,1.,0.));
#29667=DIRECTION('center_axis',(0.479172366105871,0.,-0.877720823246493));
#29668=DIRECTION('ref_axis',(-0.877720823246493,0.,-0.479172366105871));
#29669=DIRECTION('',(0.,1.,0.));
#29670=DIRECTION('center_axis',(0.533692509635919,0.,-0.845678606302959));
#29671=DIRECTION('ref_axis',(-0.845678606302959,0.,-0.533692509635919));
#29672=DIRECTION('',(0.,1.,0.));
#29673=DIRECTION('center_axis',(0.583265564466523,0.,-0.812281528355501));
#29674=DIRECTION('ref_axis',(-0.812281528355501,0.,-0.583265564466523));
#29675=DIRECTION('',(0.,1.,0.));
#29676=DIRECTION('center_axis',(0.999753136412051,0.,-0.0222186010871084));
#29677=DIRECTION('ref_axis',(-0.0222186010871084,0.,-0.99975313641205));
#29678=DIRECTION('',(0.,1.,0.));
#29679=DIRECTION('center_axis',(0.999972569709232,0.,-0.00740674213917775));
#29680=DIRECTION('ref_axis',(-0.00740674213917775,0.,-0.999972569709231));
#29681=DIRECTION('',(0.,1.,0.));
#29682=DIRECTION('center_axis',(0.999972569709232,0.,0.00740674213917775));
#29683=DIRECTION('ref_axis',(0.00740674213917775,0.,-0.999972569709231));
#29684=DIRECTION('',(0.,1.,0.));
#29685=DIRECTION('center_axis',(0.999753136412051,0.,0.0222186010871084));
#29686=DIRECTION('ref_axis',(0.0222186010871084,0.,-0.99975313641205));
#29687=DIRECTION('',(0.,1.,0.));
#29688=DIRECTION('center_axis',(0.583265564466523,0.,0.812281528355501));
#29689=DIRECTION('ref_axis',(0.812281528355501,0.,-0.583265564466523));
#29690=DIRECTION('',(0.,1.,0.));
#29691=DIRECTION('center_axis',(0.533692509635919,0.,0.845678606302959));
#29692=DIRECTION('ref_axis',(0.845678606302959,0.,-0.533692509635919));
#29693=DIRECTION('',(0.,1.,0.));
#29694=DIRECTION('center_axis',(0.479172366105871,0.,0.877720823246493));
#29695=DIRECTION('ref_axis',(0.877720823246493,0.,-0.479172366105871));
#29696=DIRECTION('',(0.,1.,0.));
#29697=DIRECTION('center_axis',(0.418575680773333,0.,0.908181919807447));
#29698=DIRECTION('ref_axis',(0.908181919807447,0.,-0.418575680773333));
#29699=DIRECTION('',(0.,1.,0.));
#29700=DIRECTION('center_axis',(0.350061695092817,0.,0.936726646161378));
#29701=DIRECTION('ref_axis',(0.936726646161378,0.,-0.350061695092817));
#29702=DIRECTION('',(0.,1.,0.));
#29703=DIRECTION('center_axis',(0.270257320503069,0.,0.962788128673439));
#29704=DIRECTION('ref_axis',(0.962788128673439,0.,-0.270257320503069));
#29705=DIRECTION('',(0.,1.,0.));
#29706=DIRECTION('center_axis',(0.171533747319284,0.,0.985178244547962));
#29707=DIRECTION('ref_axis',(0.985178244547962,0.,-0.171533747319284));
#29708=DIRECTION('center_axis',(0.977941578718451,0.,0.208878597787478));
#29709=DIRECTION('ref_axis',(0.208878597787478,0.,-0.977941578718451));
#29710=DIRECTION('',(0.,1.,0.));
#29711=DIRECTION('center_axis',(0.951361549480978,0.,0.308076617368396));
#29712=DIRECTION('ref_axis',(0.308076617368396,0.,-0.951361549480978));
#29713=DIRECTION('',(0.,1.,0.));
#29714=DIRECTION('center_axis',(0.356521352096954,0.,-0.934287175069293));
#29715=DIRECTION('ref_axis',(-0.934287175069293,0.,-0.356521352096954));
#29716=DIRECTION('',(0.,1.,0.));
#29717=DIRECTION('center_axis',(0.518266720919835,0.,-0.855219039771099));
#29718=DIRECTION('ref_axis',(-0.855219039771099,0.,-0.518266720919835));
#29719=DIRECTION('center_axis',(0.771525643922912,0.,-0.636198224431141));
#29720=DIRECTION('ref_axis',(-0.636198224431141,0.,-0.771525643922912));
#29721=DIRECTION('',(0.,1.,0.));
#29722=DIRECTION('center_axis',(0.816588132859795,0.,-0.577220773424305));
#29723=DIRECTION('ref_axis',(-0.577220773424305,0.,-0.816588132859795));
#29724=DIRECTION('',(0.,1.,0.));
#29725=DIRECTION('center_axis',(0.853835853462429,0.,-0.520542347309117));
#29726=DIRECTION('ref_axis',(-0.520542347309117,0.,-0.853835853462429));
#29727=DIRECTION('',(0.,1.,0.));
#29728=DIRECTION('center_axis',(0.885030574305657,0.,-0.465532901677421));
#29729=DIRECTION('ref_axis',(-0.465532901677421,0.,-0.885030574305657));
#29730=DIRECTION('',(0.,1.,0.));
#29731=DIRECTION('center_axis',(0.911263560158428,0.,-0.411823656347455));
#29732=DIRECTION('ref_axis',(-0.411823656347455,0.,-0.911263560158428));
#29733=DIRECTION('',(0.,1.,0.));
#29734=DIRECTION('center_axis',(0.876920914189558,0.,0.480634695228039));
#29735=DIRECTION('ref_axis',(0.480634695228039,0.,-0.876920914189558));
#29736=DIRECTION('',(0.,1.,0.));
#29737=DIRECTION('center_axis',(0.869705019525391,0.,0.493571858002802));
#29738=DIRECTION('ref_axis',(0.493571858002802,0.,-0.869705019525391));
#29739=DIRECTION('',(0.,1.,0.));
#29740=DIRECTION('center_axis',(0.862298277386211,0.,0.506400711706425));
#29741=DIRECTION('ref_axis',(0.506400711706425,0.,-0.862298277386211));
#29742=DIRECTION('',(0.,1.,0.));
#29743=DIRECTION('center_axis',(0.854702313102452,0.,0.519118441184011));
#29744=DIRECTION('ref_axis',(0.519118441184011,0.,-0.854702313102452));
#29745=DIRECTION('',(0.,1.,0.));
#29746=DIRECTION('center_axis',(0.0989820318029272,0.,0.995089220813975));
#29747=DIRECTION('ref_axis',(0.995089220813975,0.,-0.0989820318029272));
#29748=DIRECTION('',(0.,1.,0.));
#29749=DIRECTION('center_axis',(0.039351968002701,0.,0.999225411313341));
#29750=DIRECTION('ref_axis',(0.99922541131334,0.,-0.039351968002701));
#29751=DIRECTION('',(0.,1.,0.));
#29752=DIRECTION('center_axis',(-0.0238849697840649,0.,0.999714713414989));
#29753=DIRECTION('ref_axis',(0.99971471341499,0.,0.0238849697840649));
#29754=DIRECTION('',(0.,1.,0.));
#29755=DIRECTION('center_axis',(-0.0915937869476553,0.,0.995796454197638));
#29756=DIRECTION('ref_axis',(0.995796454197638,0.,0.0915937869476553));
#29757=DIRECTION('',(0.,1.,0.));
#29758=DIRECTION('center_axis',(-0.165201002238466,0.,0.986259919523959));
#29759=DIRECTION('ref_axis',(0.986259919523959,0.,0.165201002238466));
#29760=DIRECTION('',(0.,1.,0.));
#29761=DIRECTION('center_axis',(-0.247344359222349,0.,0.968927638144813));
#29762=DIRECTION('ref_axis',(0.968927638144813,0.,0.247344359222349));
#29763=DIRECTION('',(0.,1.,0.));
#29764=DIRECTION('center_axis',(-0.344036539489138,0.,0.938956260693936));
#29765=DIRECTION('ref_axis',(0.938956260693936,0.,0.344036539489138));
#29766=DIRECTION('center_axis',(0.742482951693498,0.,0.669864961350055));
#29767=DIRECTION('ref_axis',(0.669864961350055,0.,-0.742482951693498));
#29768=DIRECTION('',(0.,1.,0.));
#29769=DIRECTION('center_axis',(0.669864961350055,0.,0.742482951693498));
#29770=DIRECTION('ref_axis',(0.742482951693498,0.,-0.669864961350055));
#29771=DIRECTION('',(0.,1.,0.));
#29772=DIRECTION('center_axis',(0.775900135442185,0.,-0.630855751991531));
#29773=DIRECTION('ref_axis',(-0.63085575199153,0.,-0.775900135442185));
#29774=DIRECTION('',(0.,1.,0.));
#29775=DIRECTION('center_axis',(0.876441666138186,0.,-0.481508053781991));
#29776=DIRECTION('ref_axis',(-0.481508053781991,0.,-0.876441666138186));
#29777=DIRECTION('center_axis',(0.986259919523959,0.,-0.165201002238466));
#29778=DIRECTION('ref_axis',(-0.165201002238466,0.,-0.986259919523959));
#29779=DIRECTION('',(0.,1.,0.));
#29780=DIRECTION('center_axis',(0.995796454197638,0.,-0.0915937869476482));
#29781=DIRECTION('ref_axis',(-0.0915937869476482,0.,-0.995796454197638));
#29782=DIRECTION('',(0.,1.,0.));
#29783=DIRECTION('center_axis',(0.999714713414989,0.,-0.0238849697840649));
#29784=DIRECTION('ref_axis',(-0.0238849697840649,0.,-0.99971471341499));
#29785=DIRECTION('',(0.,1.,0.));
#29786=DIRECTION('center_axis',(0.999225411313341,0.,0.0393519680027008));
#29787=DIRECTION('ref_axis',(0.0393519680027008,0.,-0.999225411313341));
#29788=DIRECTION('',(0.,1.,0.));
#29789=DIRECTION('center_axis',(0.995089220813976,0.,0.0989820318029246));
#29790=DIRECTION('ref_axis',(0.0989820318029246,0.,-0.995089220813976));
#29791=DIRECTION('',(0.,1.,0.));
#29792=DIRECTION('center_axis',(0.519118441184015,0.,0.85470231310245));
#29793=DIRECTION('ref_axis',(0.85470231310245,0.,-0.519118441184015));
#29794=DIRECTION('',(0.,1.,0.));
#29795=DIRECTION('center_axis',(0.506400711706423,0.,0.862298277386212));
#29796=DIRECTION('ref_axis',(0.862298277386212,0.,-0.506400711706423));
#29797=DIRECTION('',(0.,1.,0.));
#29798=DIRECTION('center_axis',(0.493571858002813,0.,0.869705019525386));
#29799=DIRECTION('ref_axis',(0.869705019525386,0.,-0.493571858002812));
#29800=DIRECTION('',(0.,1.,0.));
#29801=DIRECTION('center_axis',(0.480634695228032,0.,0.876920914189562));
#29802=DIRECTION('ref_axis',(0.876920914189562,0.,-0.480634695228032));
#29803=DIRECTION('',(0.,1.,0.));
#29804=DIRECTION('center_axis',(-0.411823656347449,0.,0.911263560158431));
#29805=DIRECTION('ref_axis',(0.911263560158431,0.,0.411823656347449));
#29806=DIRECTION('',(0.,1.,0.));
#29807=DIRECTION('center_axis',(-0.465532901677421,0.,0.885030574305657));
#29808=DIRECTION('ref_axis',(0.885030574305657,0.,0.465532901677421));
#29809=DIRECTION('',(0.,1.,0.));
#29810=DIRECTION('center_axis',(-0.520542347309119,0.,0.853835853462428));
#29811=DIRECTION('ref_axis',(0.853835853462428,0.,0.520542347309119));
#29812=DIRECTION('',(0.,1.,0.));
#29813=DIRECTION('center_axis',(-0.577220773424304,0.,0.816588132859796));
#29814=DIRECTION('ref_axis',(0.816588132859796,0.,0.577220773424304));
#29815=DIRECTION('',(0.,1.,0.));
#29816=DIRECTION('center_axis',(-0.63619822443114,0.,0.771525643922913));
#29817=DIRECTION('ref_axis',(0.771525643922913,0.,0.63619822443114));
#29818=DIRECTION('',(0.,1.,0.));
#29819=DIRECTION('center_axis',(-0.698670317641747,0.,0.715443769451087));
#29820=DIRECTION('ref_axis',(0.715443769451087,0.,0.698670317641747));
#29821=DIRECTION('',(0.,1.,0.));
#29822=DIRECTION('center_axis',(-0.767422513374647,0.,0.641141705058827));
#29823=DIRECTION('ref_axis',(0.641141705058827,0.,0.767422513374647));
#29824=DIRECTION('center_axis',(0.308076617368396,0.,0.951361549480978));
#29825=DIRECTION('ref_axis',(0.951361549480978,0.,-0.308076617368396));
#29826=DIRECTION('',(0.,1.,0.));
#29827=DIRECTION('center_axis',(0.208878597787478,0.,0.977941578718451));
#29828=DIRECTION('ref_axis',(0.977941578718451,0.,-0.208878597787478));
#29829=DIRECTION('',(0.,1.,0.));
#29830=DIRECTION('center_axis',(0.987377104088484,0.,-0.158387039627108));
#29831=DIRECTION('ref_axis',(-0.158387039627108,0.,-0.987377104088484));
#29832=DIRECTION('',(0.,1.,0.));
#29833=DIRECTION('center_axis',(0.999774774701824,0.,0.0212226263670855));
#29834=DIRECTION('ref_axis',(0.0212226263670855,0.,-0.999774774701824));
#29835=DIRECTION('center_axis',(0.936726646161378,0.,0.350061695092817));
#29836=DIRECTION('ref_axis',(0.350061695092817,0.,-0.936726646161378));
#29837=DIRECTION('',(0.,1.,0.));
#29838=DIRECTION('center_axis',(0.908181919807446,0.,0.418575680773335));
#29839=DIRECTION('ref_axis',(0.418575680773335,0.,-0.908181919807446));
#29840=DIRECTION('',(0.,1.,0.));
#29841=DIRECTION('center_axis',(0.877720823246492,0.,0.479172366105872));
#29842=DIRECTION('ref_axis',(0.479172366105872,0.,-0.877720823246493));
#29843=DIRECTION('',(0.,1.,0.));
#29844=DIRECTION('center_axis',(0.845678606302959,0.,0.533692509635919));
#29845=DIRECTION('ref_axis',(0.533692509635919,0.,-0.845678606302959));
#29846=DIRECTION('',(0.,1.,0.));
#29847=DIRECTION('center_axis',(0.812281528355501,0.,0.583265564466523));
#29848=DIRECTION('ref_axis',(0.583265564466523,0.,-0.812281528355501));
#29849=DIRECTION('',(0.,1.,0.));
#29850=DIRECTION('center_axis',(0.0222186010871084,0.,0.999753136412051));
#29851=DIRECTION('ref_axis',(0.99975313641205,0.,-0.0222186010871084));
#29852=DIRECTION('',(0.,1.,0.));
#29853=DIRECTION('center_axis',(0.00740674213917776,0.,0.999972569709231));
#29854=DIRECTION('ref_axis',(0.999972569709231,0.,-0.00740674213917776));
#29855=DIRECTION('',(0.,1.,0.));
#29856=DIRECTION('center_axis',(-0.00740674213917776,0.,0.999972569709231));
#29857=DIRECTION('ref_axis',(0.999972569709231,0.,0.00740674213917776));
#29858=DIRECTION('',(0.,1.,0.));
#29859=DIRECTION('center_axis',(-0.0222186010871085,0.,0.999753136412051));
#29860=DIRECTION('ref_axis',(0.99975313641205,0.,0.0222186010871085));
#29861=DIRECTION('',(0.,1.,0.));
#29862=DIRECTION('center_axis',(-0.812281528355501,0.,0.583265564466523));
#29863=DIRECTION('ref_axis',(0.583265564466523,0.,0.812281528355501));
#29864=DIRECTION('',(0.,1.,0.));
#29865=DIRECTION('center_axis',(-0.845678606302959,0.,0.533692509635919));
#29866=DIRECTION('ref_axis',(0.533692509635919,0.,0.845678606302959));
#29867=DIRECTION('',(0.,1.,0.));
#29868=DIRECTION('center_axis',(-0.877720823246492,0.,0.479172366105872));
#29869=DIRECTION('ref_axis',(0.479172366105872,0.,0.877720823246493));
#29870=DIRECTION('',(0.,1.,0.));
#29871=DIRECTION('center_axis',(-0.908181919807446,0.,0.418575680773336));
#29872=DIRECTION('ref_axis',(0.418575680773336,0.,0.908181919807446));
#29873=DIRECTION('',(0.,1.,0.));
#29874=DIRECTION('center_axis',(-0.936726646161378,0.,0.350061695092817));
#29875=DIRECTION('ref_axis',(0.350061695092817,0.,0.936726646161378));
#29876=DIRECTION('',(0.,1.,0.));
#29877=DIRECTION('center_axis',(-0.962788128673439,0.,0.270257320503068));
#29878=DIRECTION('ref_axis',(0.270257320503068,0.,0.962788128673439));
#29879=DIRECTION('',(0.,1.,0.));
#29880=DIRECTION('center_axis',(-0.985178244547962,0.,0.171533747319286));
#29881=DIRECTION('ref_axis',(0.171533747319286,0.,0.985178244547962));
#29882=DIRECTION('center_axis',(-0.208878597787479,0.,0.977941578718451));
#29883=DIRECTION('ref_axis',(0.977941578718451,0.,0.208878597787479));
#29884=DIRECTION('',(0.,1.,0.));
#29885=DIRECTION('center_axis',(-0.308076617368397,0.,0.951361549480978));
#29886=DIRECTION('ref_axis',(0.951361549480978,0.,0.308076617368397));
#29887=DIRECTION('',(0.,1.,0.));
#29888=DIRECTION('center_axis',(0.934287175069293,0.,0.356521352096954));
#29889=DIRECTION('ref_axis',(0.356521352096954,0.,-0.934287175069293));
#29890=DIRECTION('',(0.,1.,0.));
#29891=DIRECTION('center_axis',(0.8552190397711,0.,0.518266720919834));
#29892=DIRECTION('ref_axis',(0.518266720919834,0.,-0.8552190397711));
#29893=DIRECTION('center_axis',(0.636198224431142,0.,0.771525643922911));
#29894=DIRECTION('ref_axis',(0.771525643922911,0.,-0.636198224431142));
#29895=DIRECTION('',(0.,1.,0.));
#29896=DIRECTION('center_axis',(0.577220773424306,0.,0.816588132859795));
#29897=DIRECTION('ref_axis',(0.816588132859795,0.,-0.577220773424306));
#29898=DIRECTION('',(0.,1.,0.));
#29899=DIRECTION('center_axis',(0.520542347309119,0.,0.853835853462428));
#29900=DIRECTION('ref_axis',(0.853835853462428,0.,-0.520542347309119));
#29901=DIRECTION('',(0.,1.,0.));
#29902=DIRECTION('center_axis',(0.46553290167742,0.,0.885030574305657));
#29903=DIRECTION('ref_axis',(0.885030574305657,0.,-0.46553290167742));
#29904=DIRECTION('',(0.,1.,0.));
#29905=DIRECTION('center_axis',(0.411823656347453,0.,0.911263560158429));
#29906=DIRECTION('ref_axis',(0.911263560158429,0.,-0.411823656347453));
#29907=DIRECTION('',(0.,1.,0.));
#29908=DIRECTION('center_axis',(-0.48063469522804,0.,0.876920914189557));
#29909=DIRECTION('ref_axis',(0.876920914189557,0.,0.48063469522804));
#29910=DIRECTION('',(0.,1.,0.));
#29911=DIRECTION('center_axis',(-0.493571858002805,0.,0.86970501952539));
#29912=DIRECTION('ref_axis',(0.86970501952539,0.,0.493571858002805));
#29913=DIRECTION('',(0.,1.,0.));
#29914=DIRECTION('center_axis',(-0.506400711706427,0.,0.86229827738621));
#29915=DIRECTION('ref_axis',(0.86229827738621,0.,0.506400711706427));
#29916=DIRECTION('',(0.,1.,0.));
#29917=DIRECTION('center_axis',(-0.519118441184015,0.,0.85470231310245));
#29918=DIRECTION('ref_axis',(0.85470231310245,0.,0.519118441184015));
#29919=DIRECTION('',(0.,1.,0.));
#29920=DIRECTION('center_axis',(-0.995089220813975,0.,0.0989820318029307));
#29921=DIRECTION('ref_axis',(0.0989820318029307,0.,0.995089220813975));
#29922=DIRECTION('',(0.,1.,0.));
#29923=DIRECTION('center_axis',(-0.999225411313341,0.,0.0393519680026976));
#29924=DIRECTION('ref_axis',(0.0393519680026975,0.,0.999225411313341));
#29925=DIRECTION('',(0.,1.,0.));
#29926=DIRECTION('center_axis',(-0.99971471341499,0.,-0.0238849697840614));
#29927=DIRECTION('ref_axis',(-0.0238849697840614,0.,0.99971471341499));
#29928=DIRECTION('',(0.,1.,0.));
#29929=DIRECTION('center_axis',(-0.995796454197637,0.,-0.0915937869476591));
#29930=DIRECTION('ref_axis',(-0.0915937869476591,0.,0.995796454197637));
#29931=DIRECTION('',(0.,1.,0.));
#29932=DIRECTION('center_axis',(-0.98625991952396,0.,-0.165201002238462));
#29933=DIRECTION('ref_axis',(-0.165201002238462,0.,0.98625991952396));
#29934=DIRECTION('',(0.,1.,0.));
#29935=DIRECTION('center_axis',(-0.968927638144813,0.,-0.247344359222349));
#29936=DIRECTION('ref_axis',(-0.247344359222349,0.,0.968927638144813));
#29937=DIRECTION('',(0.,1.,0.));
#29938=DIRECTION('center_axis',(-0.938956260693934,0.,-0.344036539489144));
#29939=DIRECTION('ref_axis',(-0.344036539489144,0.,0.938956260693934));
#29940=DIRECTION('center_axis',(-0.669864961350055,0.,0.742482951693498));
#29941=DIRECTION('ref_axis',(0.742482951693498,0.,0.669864961350055));
#29942=DIRECTION('',(0.,1.,0.));
#29943=DIRECTION('center_axis',(-0.742482951693498,0.,0.669864961350055));
#29944=DIRECTION('ref_axis',(0.669864961350055,0.,0.742482951693498));
#29945=DIRECTION('',(0.,1.,0.));
#29946=DIRECTION('center_axis',(0.630855751991531,0.,0.775900135442185));
#29947=DIRECTION('ref_axis',(0.775900135442185,0.,-0.63085575199153));
#29948=DIRECTION('',(0.,1.,0.));
#29949=DIRECTION('center_axis',(0.48150805378198,0.,0.876441666138192));
#29950=DIRECTION('ref_axis',(0.876441666138192,0.,-0.48150805378198));
#29951=DIRECTION('center_axis',(0.165201002238459,0.,0.98625991952396));
#29952=DIRECTION('ref_axis',(0.98625991952396,0.,-0.165201002238459));
#29953=DIRECTION('',(0.,1.,0.));
#29954=DIRECTION('center_axis',(0.0915937869476627,0.,0.995796454197637));
#29955=DIRECTION('ref_axis',(0.995796454197637,0.,-0.0915937869476627));
#29956=DIRECTION('',(0.,1.,0.));
#29957=DIRECTION('center_axis',(0.0238849697840613,0.,0.99971471341499));
#29958=DIRECTION('ref_axis',(0.99971471341499,0.,-0.0238849697840613));
#29959=DIRECTION('',(0.,1.,0.));
#29960=DIRECTION('center_axis',(-0.0393519680026977,0.,0.999225411313341));
#29961=DIRECTION('ref_axis',(0.999225411313341,0.,0.0393519680026977));
#29962=DIRECTION('',(0.,1.,0.));
#29963=DIRECTION('center_axis',(-0.0989820318029304,0.,0.995089220813975));
#29964=DIRECTION('ref_axis',(0.995089220813975,0.,0.0989820318029304));
#29965=DIRECTION('',(0.,1.,0.));
#29966=DIRECTION('center_axis',(-0.854702313102456,0.,0.519118441184006));
#29967=DIRECTION('ref_axis',(0.519118441184006,0.,0.854702313102456));
#29968=DIRECTION('',(0.,1.,0.));
#29969=DIRECTION('center_axis',(-0.862298277386207,0.,0.506400711706431));
#29970=DIRECTION('ref_axis',(0.506400711706431,0.,0.862298277386207));
#29971=DIRECTION('',(0.,1.,0.));
#29972=DIRECTION('center_axis',(-0.869705019525391,0.,0.493571858002802));
#29973=DIRECTION('ref_axis',(0.493571858002802,0.,0.869705019525391));
#29974=DIRECTION('',(0.,1.,0.));
#29975=DIRECTION('center_axis',(-0.876920914189556,0.,0.480634695228042));
#29976=DIRECTION('ref_axis',(0.480634695228042,0.,0.876920914189556));
#29977=DIRECTION('',(0.,1.,0.));
#29978=DIRECTION('center_axis',(-0.91126356015843,0.,-0.41182365634745));
#29979=DIRECTION('ref_axis',(-0.41182365634745,0.,0.91126356015843));
#29980=DIRECTION('',(0.,1.,0.));
#29981=DIRECTION('center_axis',(-0.885030574305655,0.,-0.465532901677425));
#29982=DIRECTION('ref_axis',(-0.465532901677425,0.,0.885030574305655));
#29983=DIRECTION('',(0.,1.,0.));
#29984=DIRECTION('center_axis',(-0.85383585346243,0.,-0.520542347309115));
#29985=DIRECTION('ref_axis',(-0.520542347309115,0.,0.85383585346243));
#29986=DIRECTION('',(0.,1.,0.));
#29987=DIRECTION('center_axis',(-0.816588132859791,0.,-0.577220773424311));
#29988=DIRECTION('ref_axis',(-0.577220773424311,0.,0.816588132859791));
#29989=DIRECTION('',(0.,1.,0.));
#29990=DIRECTION('center_axis',(-0.771525643922916,0.,-0.636198224431136));
#29991=DIRECTION('ref_axis',(-0.636198224431136,0.,0.771525643922916));
#29992=DIRECTION('',(0.,1.,0.));
#29993=DIRECTION('center_axis',(-0.715443769451087,0.,-0.698670317641747));
#29994=DIRECTION('ref_axis',(-0.698670317641747,0.,0.715443769451087));
#29995=DIRECTION('',(0.,1.,0.));
#29996=DIRECTION('center_axis',(-0.641141705058821,0.,-0.767422513374652));
#29997=DIRECTION('ref_axis',(-0.767422513374652,0.,0.641141705058821));
#29998=DIRECTION('center_axis',(-0.951361549480978,0.,0.308076617368396));
#29999=DIRECTION('ref_axis',(0.308076617368396,0.,0.951361549480978));
#30000=DIRECTION('',(0.,1.,0.));
#30001=DIRECTION('center_axis',(-0.977941578718451,0.,0.20887859778748));
#30002=DIRECTION('ref_axis',(0.20887859778748,0.,0.977941578718451));
#30003=DIRECTION('',(0.,1.,0.));
#30004=DIRECTION('center_axis',(0.158387039627109,0.,0.987377104088484));
#30005=DIRECTION('ref_axis',(0.987377104088484,0.,-0.158387039627109));
#30006=DIRECTION('',(0.,1.,0.));
#30007=DIRECTION('center_axis',(-0.0212226263670972,0.,0.999774774701824));
#30008=DIRECTION('ref_axis',(0.999774774701824,0.,0.0212226263670972));
#30009=DIRECTION('center_axis',(-0.350061695092823,0.,0.936726646161376));
#30010=DIRECTION('ref_axis',(0.936726646161376,0.,0.350061695092823));
#30011=DIRECTION('',(0.,1.,0.));
#30012=DIRECTION('center_axis',(-0.418575680773325,0.,0.908181919807451));
#30013=DIRECTION('ref_axis',(0.908181919807451,0.,0.418575680773325));
#30014=DIRECTION('',(0.,1.,0.));
#30015=DIRECTION('center_axis',(-0.479172366105876,0.,0.87772082324649));
#30016=DIRECTION('ref_axis',(0.87772082324649,0.,0.479172366105876));
#30017=DIRECTION('',(0.,1.,0.));
#30018=DIRECTION('center_axis',(-0.533692509635917,0.,0.84567860630296));
#30019=DIRECTION('ref_axis',(0.84567860630296,0.,0.533692509635917));
#30020=DIRECTION('',(0.,1.,0.));
#30021=DIRECTION('center_axis',(-0.583265564466524,0.,0.8122815283555));
#30022=DIRECTION('ref_axis',(0.8122815283555,0.,0.583265564466524));
#30023=DIRECTION('',(0.,1.,0.));
#30024=DIRECTION('center_axis',(-0.999753136412051,0.,0.0222186010871084));
#30025=DIRECTION('ref_axis',(0.0222186010871084,0.,0.99975313641205));
#30026=DIRECTION('',(0.,1.,0.));
#30027=DIRECTION('center_axis',(-0.999972569709231,0.,0.00740674213917776));
#30028=DIRECTION('ref_axis',(0.00740674213917776,0.,0.999972569709231));
#30029=DIRECTION('',(0.,1.,0.));
#30030=DIRECTION('center_axis',(-0.999972569709231,0.,-0.00740674213917776));
#30031=DIRECTION('ref_axis',(-0.00740674213917776,0.,0.999972569709231));
#30032=DIRECTION('',(0.,1.,0.));
#30033=DIRECTION('center_axis',(-0.999753136412051,0.,-0.0222186010871084));
#30034=DIRECTION('ref_axis',(-0.0222186010871084,0.,0.99975313641205));
#30035=DIRECTION('',(0.,1.,0.));
#30036=DIRECTION('center_axis',(-0.583265564466527,0.,-0.812281528355498));
#30037=DIRECTION('ref_axis',(-0.812281528355498,0.,0.583265564466527));
#30038=DIRECTION('',(0.,1.,0.));
#30039=DIRECTION('center_axis',(-0.533692509635915,0.,-0.845678606302962));
#30040=DIRECTION('ref_axis',(-0.845678606302961,0.,0.533692509635915));
#30041=DIRECTION('',(0.,1.,0.));
#30042=DIRECTION('center_axis',(-0.479172366105876,0.,-0.87772082324649));
#30043=DIRECTION('ref_axis',(-0.87772082324649,0.,0.479172366105876));
#30044=DIRECTION('',(0.,1.,0.));
#30045=DIRECTION('center_axis',(-0.418575680773326,0.,-0.908181919807451));
#30046=DIRECTION('ref_axis',(-0.908181919807451,0.,0.418575680773326));
#30047=DIRECTION('',(0.,1.,0.));
#30048=DIRECTION('center_axis',(-0.350061695092823,0.,-0.936726646161376));
#30049=DIRECTION('ref_axis',(-0.936726646161376,0.,0.350061695092823));
#30050=DIRECTION('',(0.,1.,0.));
#30051=DIRECTION('center_axis',(-0.270257320503067,0.,-0.962788128673439));
#30052=DIRECTION('ref_axis',(-0.962788128673439,0.,0.270257320503067));
#30053=DIRECTION('',(0.,1.,0.));
#30054=DIRECTION('center_axis',(-0.171533747319281,0.,-0.985178244547963));
#30055=DIRECTION('ref_axis',(-0.985178244547962,0.,0.171533747319281));
#30056=DIRECTION('center_axis',(-0.977941578718451,0.,-0.208878597787478));
#30057=DIRECTION('ref_axis',(-0.208878597787478,0.,0.977941578718451));
#30058=DIRECTION('',(0.,1.,0.));
#30059=DIRECTION('center_axis',(-0.951361549480978,0.,-0.308076617368396));
#30060=DIRECTION('ref_axis',(-0.308076617368396,0.,0.951361549480978));
#30061=DIRECTION('',(0.,1.,0.));
#30062=DIRECTION('center_axis',(-0.356521352096954,0.,0.934287175069293));
#30063=DIRECTION('ref_axis',(0.934287175069293,0.,0.356521352096954));
#30064=DIRECTION('',(0.,1.,0.));
#30065=DIRECTION('center_axis',(-0.518266720919843,0.,0.855219039771095));
#30066=DIRECTION('ref_axis',(0.855219039771095,0.,0.518266720919843));
#30067=DIRECTION('center_axis',(-0.771525643922917,0.,0.636198224431135));
#30068=DIRECTION('ref_axis',(0.636198224431135,0.,0.771525643922917));
#30069=DIRECTION('',(0.,1.,0.));
#30070=DIRECTION('center_axis',(-0.81658813285979,0.,0.577220773424313));
#30071=DIRECTION('ref_axis',(0.577220773424313,0.,0.81658813285979));
#30072=DIRECTION('',(0.,1.,0.));
#30073=DIRECTION('center_axis',(-0.85383585346243,0.,0.520542347309115));
#30074=DIRECTION('ref_axis',(0.520542347309115,0.,0.85383585346243));
#30075=DIRECTION('',(0.,1.,0.));
#30076=DIRECTION('center_axis',(-0.885030574305656,0.,0.465532901677422));
#30077=DIRECTION('ref_axis',(0.465532901677422,0.,0.885030574305656));
#30078=DIRECTION('',(0.,1.,0.));
#30079=DIRECTION('center_axis',(-0.911263560158432,0.,0.411823656347447));
#30080=DIRECTION('ref_axis',(0.411823656347447,0.,0.911263560158432));
#30081=DIRECTION('',(0.,1.,0.));
#30082=DIRECTION('center_axis',(-0.876920914189563,0.,-0.48063469522803));
#30083=DIRECTION('ref_axis',(-0.48063469522803,0.,0.876920914189563));
#30084=DIRECTION('',(0.,1.,0.));
#30085=DIRECTION('center_axis',(-0.869705019525385,0.,-0.493571858002814));
#30086=DIRECTION('ref_axis',(-0.493571858002814,0.,0.869705019525385));
#30087=DIRECTION('',(0.,1.,0.));
#30088=DIRECTION('center_axis',(-0.862298277386214,0.,-0.506400711706419));
#30089=DIRECTION('ref_axis',(-0.506400711706419,0.,0.862298277386214));
#30090=DIRECTION('',(0.,1.,0.));
#30091=DIRECTION('center_axis',(-0.854702313102448,0.,-0.519118441184019));
#30092=DIRECTION('ref_axis',(-0.519118441184019,0.,0.854702313102448));
#30093=DIRECTION('',(0.,1.,0.));
#30094=DIRECTION('center_axis',(-0.0989820318029307,0.,-0.995089220813975));
#30095=DIRECTION('ref_axis',(-0.995089220813975,0.,0.0989820318029307));
#30096=DIRECTION('',(0.,1.,0.));
#30097=DIRECTION('center_axis',(-0.0393519680026942,0.,-0.999225411313341));
#30098=DIRECTION('ref_axis',(-0.999225411313341,0.,0.0393519680026942));
#30099=DIRECTION('',(0.,1.,0.));
#30100=DIRECTION('center_axis',(0.023884969784058,0.,-0.99971471341499));
#30101=DIRECTION('ref_axis',(-0.99971471341499,0.,-0.023884969784058));
#30102=DIRECTION('',(0.,1.,0.));
#30103=DIRECTION('center_axis',(0.091593786947663,0.,-0.995796454197637));
#30104=DIRECTION('ref_axis',(-0.995796454197637,0.,-0.091593786947663));
#30105=DIRECTION('',(0.,1.,0.));
#30106=DIRECTION('center_axis',(0.165201002238458,0.,-0.986259919523961));
#30107=DIRECTION('ref_axis',(-0.986259919523961,0.,-0.165201002238458));
#30108=DIRECTION('',(0.,1.,0.));
#30109=DIRECTION('center_axis',(0.247344359222354,0.,-0.968927638144812));
#30110=DIRECTION('ref_axis',(-0.968927638144812,0.,-0.247344359222354));
#30111=DIRECTION('',(0.,1.,0.));
#30112=DIRECTION('center_axis',(0.344036539489142,0.,-0.938956260693935));
#30113=DIRECTION('ref_axis',(-0.938956260693935,0.,-0.344036539489142));
#30114=DIRECTION('center_axis',(-0.742482951693499,0.,-0.669864961350053));
#30115=DIRECTION('ref_axis',(-0.669864961350053,0.,0.742482951693499));
#30116=DIRECTION('',(0.,1.,0.));
#30117=DIRECTION('center_axis',(-0.669864961350055,0.,-0.742482951693498));
#30118=DIRECTION('ref_axis',(-0.742482951693498,0.,0.669864961350055));
#30119=DIRECTION('',(0.,1.,0.));
#30120=DIRECTION('center_axis',(-0.775900135442185,0.,0.630855751991531));
#30121=DIRECTION('ref_axis',(0.630855751991531,0.,0.775900135442185));
#30122=DIRECTION('',(0.,1.,0.));
#30123=DIRECTION('center_axis',(-0.876441666138186,0.,0.481508053781991));
#30124=DIRECTION('ref_axis',(0.481508053781991,0.,0.876441666138186));
#30125=DIRECTION('center_axis',(-0.986259919523958,0.,0.165201002238474));
#30126=DIRECTION('ref_axis',(0.165201002238474,0.,0.986259919523958));
#30127=DIRECTION('',(0.,1.,0.));
#30128=DIRECTION('center_axis',(-0.995796454197638,0.,0.0915937869476479));
#30129=DIRECTION('ref_axis',(0.0915937869476479,0.,0.995796454197638));
#30130=DIRECTION('',(0.,1.,0.));
#30131=DIRECTION('center_axis',(-0.999714713414989,0.,0.0238849697840824));
#30132=DIRECTION('ref_axis',(0.0238849697840824,0.,0.999714713414989));
#30133=DIRECTION('',(0.,1.,0.));
#30134=DIRECTION('center_axis',(-0.99922541131334,0.,-0.0393519680027076));
#30135=DIRECTION('ref_axis',(-0.0393519680027076,0.,0.99922541131334));
#30136=DIRECTION('',(0.,1.,0.));
#30137=DIRECTION('center_axis',(-0.995089220813975,0.,-0.0989820318029304));
#30138=DIRECTION('ref_axis',(-0.0989820318029304,0.,0.995089220813975));
#30139=DIRECTION('',(0.,1.,0.));
#30140=DIRECTION('center_axis',(-0.51911844118402,0.,-0.854702313102447));
#30141=DIRECTION('ref_axis',(-0.854702313102447,0.,0.51911844118402));
#30142=DIRECTION('',(0.,1.,0.));
#30143=DIRECTION('center_axis',(-0.506400711706418,0.,-0.862298277386215));
#30144=DIRECTION('ref_axis',(-0.862298277386214,0.,0.506400711706418));
#30145=DIRECTION('',(0.,1.,0.));
#30146=DIRECTION('center_axis',(-0.493571858002809,0.,-0.869705019525388));
#30147=DIRECTION('ref_axis',(-0.869705019525388,0.,0.493571858002809));
#30148=DIRECTION('',(0.,1.,0.));
#30149=DIRECTION('center_axis',(-0.480634695228043,0.,-0.876920914189556));
#30150=DIRECTION('ref_axis',(-0.876920914189556,0.,0.480634695228043));
#30151=DIRECTION('',(0.,1.,0.));
#30152=DIRECTION('center_axis',(0.411823656347446,0.,-0.911263560158432));
#30153=DIRECTION('ref_axis',(-0.911263560158432,0.,-0.411823656347446));
#30154=DIRECTION('',(0.,1.,0.));
#30155=DIRECTION('center_axis',(0.465532901677419,0.,-0.885030574305658));
#30156=DIRECTION('ref_axis',(-0.885030574305658,0.,-0.465532901677419));
#30157=DIRECTION('',(0.,1.,0.));
#30158=DIRECTION('center_axis',(0.520542347309132,0.,-0.85383585346242));
#30159=DIRECTION('ref_axis',(-0.85383585346242,0.,-0.520542347309132));
#30160=DIRECTION('',(0.,1.,0.));
#30161=DIRECTION('center_axis',(0.577220773424303,0.,-0.816588132859797));
#30162=DIRECTION('ref_axis',(-0.816588132859797,0.,-0.577220773424303));
#30163=DIRECTION('',(0.,1.,0.));
#30164=DIRECTION('center_axis',(0.636198224431145,0.,-0.771525643922909));
#30165=DIRECTION('ref_axis',(-0.771525643922909,0.,-0.636198224431145));
#30166=DIRECTION('',(0.,1.,0.));
#30167=DIRECTION('center_axis',(0.69867031764173,0.,-0.715443769451104));
#30168=DIRECTION('ref_axis',(-0.715443769451104,0.,-0.69867031764173));
#30169=DIRECTION('',(0.,1.,0.));
#30170=DIRECTION('center_axis',(0.767422513374652,0.,-0.641141705058821));
#30171=DIRECTION('ref_axis',(-0.641141705058821,0.,-0.767422513374652));
#30172=DIRECTION('center_axis',(-0.308076617368395,0.,-0.951361549480978));
#30173=DIRECTION('ref_axis',(-0.951361549480978,0.,0.308076617368395));
#30174=DIRECTION('center_axis',(0.,1.,0.));
#30175=DIRECTION('ref_axis',(0.,0.,1.));
#30176=DIRECTION('',(0.,-1.,0.));
#30177=DIRECTION('center_axis',(0.,1.,0.));
#30178=DIRECTION('ref_axis',(1.,0.,0.));
#30179=DIRECTION('center_axis',(0.,-1.,0.));
#30180=DIRECTION('ref_axis',(0.,0.,-1.));
#30181=DIRECTION('center_axis',(0.,1.,0.));
#30182=DIRECTION('ref_axis',(1.,0.,0.));
#30183=DIRECTION('center_axis',(0.,1.,0.));
#30184=DIRECTION('ref_axis',(0.,0.,1.));
#30185=DIRECTION('center_axis',(0.,1.,0.));
#30186=DIRECTION('ref_axis',(1.,0.,0.));
#30187=DIRECTION('',(8.65956056235491E-17,-0.707106781186549,0.707106781186546));
#30188=DIRECTION('center_axis',(0.,1.,0.));
#30189=DIRECTION('ref_axis',(0.,0.,1.));
#30190=DIRECTION('center_axis',(0.,1.,0.));
#30191=DIRECTION('ref_axis',(1.,0.,0.));
#30192=DIRECTION('',(0.,-1.,0.));
#30193=DIRECTION('center_axis',(0.,-1.,0.));
#30194=DIRECTION('ref_axis',(0.,0.,-1.));
#30195=DIRECTION('center_axis',(0.,1.,0.));
#30196=DIRECTION('ref_axis',(0.,0.,1.));
#30197=DIRECTION('center_axis',(0.,1.,0.));
#30198=DIRECTION('ref_axis',(1.,0.,0.));
#30199=DIRECTION('',(0.,-1.,0.));
#30200=DIRECTION('center_axis',(0.,1.,0.));
#30201=DIRECTION('ref_axis',(0.,0.,1.));
#30202=DIRECTION('axis',(0.,0.,1.));
#30203=DIRECTION('refdir',(1.,0.,0.));
#30204=DIRECTION('center_axis',(0.414495032230687,-0.707106781186548,-0.572882071857796));
#30205=DIRECTION('ref_axis',(-0.810177595661694,0.,-0.586184496116911));
#30206=DIRECTION('',(0.451594888615274,-0.386714295024759,0.80406101173982));
#30207=DIRECTION('',(-0.810177595661694,0.,-0.586184496116911));
#30208=DIRECTION('',(-0.384785213588102,-0.706639907076676,0.593801634496425));
#30209=DIRECTION('',(0.810177595661694,0.,0.586184496116911));
#30210=DIRECTION('',(0.681078899711059,-0.1764913880685,0.710621082086668));
#30211=DIRECTION('',(0.547096153529848,-0.309436927624307,0.777775408852244));
#30212=DIRECTION('center_axis',(0.,1.,0.));
#30213=DIRECTION('ref_axis',(1.,0.,0.));
#30214=DIRECTION('',(-0.54380964897583,0.,0.839208594856359));
#30215=DIRECTION('',(0.48969323063785,0.,0.871894798623931));
#30216=DIRECTION('',(0.414834765185058,0.,0.909896762052629));
#30217=DIRECTION('',(0.346203891732264,0.,0.938159296361463));
#30218=DIRECTION('',(0.281816316675586,0.,0.959468375536894));
#30219=DIRECTION('',(0.220607484589178,0.,0.975362669853237));
#30220=DIRECTION('',(0.161938741065869,0.,0.986800812799626));
#30221=DIRECTION('',(-0.691221298772304,0.,0.722643145766656));
#30222=DIRECTION('',(-0.701850027448819,0.,0.712324742635051));
#30223=DIRECTION('',(-0.712324742635051,0.,0.701850027448819));
#30224=DIRECTION('',(-0.722643145766653,0.,0.691221298772308));
#30225=DIRECTION('',(-0.986800812799626,0.,-0.161938741065865));
#30226=DIRECTION('',(-0.975362669853236,0.,-0.220607484589183));
#30227=DIRECTION('',(-0.959468375536896,0.,-0.28181631667558));
#30228=DIRECTION('',(-0.938159296361463,0.,-0.346203891732262));
#30229=DIRECTION('',(-0.909896762052626,0.,-0.414834765185062));
#30230=DIRECTION('',(-0.87189479862393,0.,-0.489693230637852));
#30231=DIRECTION('',(0.58618449611691,0.,0.810177595661694));
#30232=DIRECTION('',(-0.839208594856358,0.,0.543809648975832));
#30233=DIRECTION('',(-0.890557268264346,0.,0.454871137731935));
#30234=DIRECTION('',(-0.408542131361568,0.,-0.912739462772673));
#30235=DIRECTION('',(-0.011860621518292,0.,0.999929660354767));
#30236=DIRECTION('',(-0.0956909360031075,0.,0.995411093351309));
#30237=DIRECTION('',(-0.169258283051556,0.,0.985571729311692));
#30238=DIRECTION('',(-0.235674098326445,0.,0.971832145680527));
#30239=DIRECTION('',(-0.296629649007403,0.,0.954992592290508));
#30240=DIRECTION('',(-0.353157342779898,0.,0.935563942892543));
#30241=DIRECTION('',(-0.959936777257016,0.,0.280216672718478));
#30242=DIRECTION('',(-0.963982324735009,0.,0.265966309141754));
#30243=DIRECTION('',(-0.967816336590576,0.,0.251657582099957));
#30244=DIRECTION('',(-0.971437971490777,0.,0.237293631490364));
#30245=DIRECTION('',(-0.773625201826672,0.,-0.633643470019727));
#30246=DIRECTION('',(-0.734385107701324,0.,-0.678733020845837));
#30247=DIRECTION('',(-0.690015829004958,0.,-0.723794277210452));
#30248=DIRECTION('',(-0.639367837579427,0.,-0.768901013309911));
#30249=DIRECTION('',(-0.580576328166257,0.,-0.814205826049523));
#30250=DIRECTION('',(-0.510236429716897,0.,-0.860034177105627));
#30251=DIRECTION('',(0.10256186711098,0.,0.99472662747848));
#30252=DIRECTION('',(-0.998680786707765,0.,0.0513486734079894));
#30253=DIRECTION('',(-0.998680786707765,0.,-0.0513486734079893));
#30254=DIRECTION('',(0.10256186711098,0.,-0.99472662747848));
#30255=DIRECTION('',(-0.510236429716897,0.,0.860034177105627));
#30256=DIRECTION('',(-0.580576328166257,0.,0.814205826049523));
#30257=DIRECTION('',(-0.639367837579427,0.,0.768901013309911));
#30258=DIRECTION('',(-0.690015829004958,0.,0.723794277210452));
#30259=DIRECTION('',(-0.734385107701324,0.,0.678733020845836));
#30260=DIRECTION('',(-0.773625201826672,0.,0.633643470019727));
#30261=DIRECTION('',(-0.971437971490777,0.,-0.237293631490364));
#30262=DIRECTION('',(-0.967816336590576,0.,-0.251657582099957));
#30263=DIRECTION('',(-0.963982324735007,0.,-0.265966309141762));
#30264=DIRECTION('',(-0.959936777257018,0.,-0.28021667271847));
#30265=DIRECTION('',(-0.353157342779898,0.,-0.935563942892543));
#30266=DIRECTION('',(-0.296629649007399,0.,-0.954992592290509));
#30267=DIRECTION('',(-0.235674098326447,0.,-0.971832145680527));
#30268=DIRECTION('',(-0.169258283051554,0.,-0.985571729311692));
#30269=DIRECTION('',(-0.0956909360031101,0.,-0.995411093351309));
#30270=DIRECTION('',(-0.0118606215182901,0.,-0.999929660354767));
#30271=DIRECTION('',(-0.408542131361568,0.,0.912739462772673));
#30272=DIRECTION('',(-0.890557268264346,0.,-0.454871137731935));
#30273=DIRECTION('',(-0.839208594856359,0.,-0.54380964897583));
#30274=DIRECTION('',(0.586184496116912,0.,-0.810177595661693));
#30275=DIRECTION('',(-0.871894798623918,0.,0.489693230637874));
#30276=DIRECTION('',(-0.909896762052635,0.,0.414834765185043));
#30277=DIRECTION('',(-0.938159296361459,0.,0.346203891732275));
#30278=DIRECTION('',(-0.9594683755369,0.,0.281816316675565));
#30279=DIRECTION('',(-0.975362669853236,0.,0.220607484589184));
#30280=DIRECTION('',(-0.986800812799626,0.,0.161938741065868));
#30281=DIRECTION('',(-0.722643145766652,0.,-0.691221298772308));
#30282=DIRECTION('',(-0.712324742635051,0.,-0.701850027448819));
#30283=DIRECTION('',(-0.701850027448815,0.,-0.712324742635055));
#30284=DIRECTION('',(-0.691221298772312,0.,-0.722643145766649));
#30285=DIRECTION('',(0.161938741065865,0.,-0.986800812799626));
#30286=DIRECTION('',(0.220607484589187,0.,-0.975362669853235));
#30287=DIRECTION('',(0.281816316675565,0.,-0.9594683755369));
#30288=DIRECTION('',(0.346203891732272,0.,-0.93815929636146));
#30289=DIRECTION('',(0.414834765185049,0.,-0.909896762052633));
#30290=DIRECTION('',(0.489693230637868,0.,-0.871894798623921));
#30291=DIRECTION('',(-0.810177595661692,0.,0.586184496116913));
#30292=DIRECTION('',(-0.543809648975831,0.,-0.839208594856358));
#30293=DIRECTION('',(-0.454871137731934,0.,-0.890557268264347));
#30294=DIRECTION('',(0.912739462772673,0.,-0.408542131361568));
#30295=DIRECTION('',(-0.999929660354767,0.,-0.0118606215182919));
#30296=DIRECTION('',(-0.995411093351309,0.,-0.0956909360031137));
#30297=DIRECTION('',(-0.985571729311693,0.,-0.169258283051549));
#30298=DIRECTION('',(-0.971832145680526,0.,-0.235674098326448));
#30299=DIRECTION('',(-0.954992592290512,0.,-0.296629649007392));
#30300=DIRECTION('',(-0.93556394289254,0.,-0.353157342779906));
#30301=DIRECTION('',(-0.280216672718464,0.,-0.95993677725702));
#30302=DIRECTION('',(-0.265966309141754,0.,-0.963982324735009));
#30303=DIRECTION('',(-0.251657582099958,0.,-0.967816336590576));
#30304=DIRECTION('',(-0.237293631490368,0.,-0.971437971490776));
#30305=DIRECTION('',(0.633643470019724,0.,-0.773625201826675));
#30306=DIRECTION('',(0.678733020845843,0.,-0.734385107701318));
#30307=DIRECTION('',(0.723794277210445,0.,-0.690015829004965));
#30308=DIRECTION('',(0.768901013309918,0.,-0.639367837579419));
#30309=DIRECTION('',(0.814205826049519,0.,-0.580576328166263));
#30310=DIRECTION('',(0.86003417710563,0.,-0.510236429716893));
#30311=DIRECTION('',(-0.99472662747848,0.,0.102561867110979));
#30312=DIRECTION('',(-0.0513486734079878,0.,-0.998680786707765));
#30313=DIRECTION('',(0.0513486734079878,0.,-0.998680786707765));
#30314=DIRECTION('',(0.99472662747848,0.,0.102561867110979));
#30315=DIRECTION('',(-0.86003417710563,0.,-0.510236429716893));
#30316=DIRECTION('',(-0.814205826049522,0.,-0.580576328166259));
#30317=DIRECTION('',(-0.768901013309911,0.,-0.639367837579427));
#30318=DIRECTION('',(-0.723794277210454,0.,-0.690015829004956));
#30319=DIRECTION('',(-0.678733020845838,0.,-0.734385107701322));
#30320=DIRECTION('',(-0.63364347001972,0.,-0.773625201826678));
#30321=DIRECTION('',(0.237293631490357,0.,-0.971437971490779));
#30322=DIRECTION('',(0.251657582099958,0.,-0.967816336590576));
#30323=DIRECTION('',(0.265966309141754,0.,-0.963982324735009));
#30324=DIRECTION('',(0.280216672718478,0.,-0.959936777257016));
#30325=DIRECTION('',(0.935563942892542,0.,-0.3531573427799));
#30326=DIRECTION('',(0.95499259229051,0.,-0.296629649007398));
#30327=DIRECTION('',(0.971832145680524,0.,-0.235674098326456));
#30328=DIRECTION('',(0.985571729311695,0.,-0.169258283051542));
#30329=DIRECTION('',(0.99541109335131,0.,-0.0956909360031057));
#30330=DIRECTION('',(0.999929660354767,0.,-0.011860621518292));
#30331=DIRECTION('',(-0.912739462772673,0.,-0.408542131361568));
#30332=DIRECTION('',(0.454871137731933,0.,-0.890557268264347));
#30333=DIRECTION('',(0.543809648975832,0.,-0.839208594856358));
#30334=DIRECTION('',(0.810177595661692,0.,0.586184496116913));
#30335=DIRECTION('',(-0.489693230637875,0.,-0.871894798623917));
#30336=DIRECTION('',(-0.414834765185046,0.,-0.909896762052634));
#30337=DIRECTION('',(-0.346203891732269,0.,-0.938159296361461));
#30338=DIRECTION('',(-0.281816316675564,0.,-0.9594683755369));
#30339=DIRECTION('',(-0.22060748458919,0.,-0.975362669853235));
#30340=DIRECTION('',(-0.161938741065865,0.,-0.986800812799626));
#30341=DIRECTION('',(0.691221298772293,0.,-0.722643145766667));
#30342=DIRECTION('',(0.701850027448823,0.,-0.712324742635048));
#30343=DIRECTION('',(0.71232474263504,0.,-0.701850027448831));
#30344=DIRECTION('',(0.722643145766668,0.,-0.691221298772292));
#30345=DIRECTION('',(0.986800812799626,0.,0.161938741065863));
#30346=DIRECTION('',(0.975362669853233,0.,0.2206074845892));
#30347=DIRECTION('',(0.959468375536898,0.,0.281816316675571));
#30348=DIRECTION('',(0.938159296361463,0.,0.346203891732263));
#30349=DIRECTION('',(0.909896762052627,0.,0.414834765185061));
#30350=DIRECTION('',(0.871894798623937,0.,0.48969323063784));
#30351=DIRECTION('',(-0.586184496116911,0.,-0.810177595661694));
#30352=DIRECTION('',(0.839208594856358,0.,-0.543809648975832));
#30353=DIRECTION('',(0.890557268264346,0.,-0.454871137731935));
#30354=DIRECTION('',(0.408542131361568,0.,0.912739462772673));
#30355=DIRECTION('',(0.0118606215182939,0.,-0.999929660354767));
#30356=DIRECTION('',(0.0956909360031021,0.,-0.99541109335131));
#30357=DIRECTION('',(0.169258283051555,0.,-0.985571729311692));
#30358=DIRECTION('',(0.235674098326432,0.,-0.97183214568053));
#30359=DIRECTION('',(0.296629649007409,0.,-0.954992592290506));
#30360=DIRECTION('',(0.3531573427799,0.,-0.935563942892542));
#30361=DIRECTION('',(0.959936777257014,0.,-0.280216672718486));
#30362=DIRECTION('',(0.963982324735007,0.,-0.265966309141761));
#30363=DIRECTION('',(0.967816336590582,0.,-0.251657582099936));
#30364=DIRECTION('',(0.971437971490773,0.,-0.237293631490379));
#30365=DIRECTION('',(0.773625201826676,0.,0.633643470019722));
#30366=DIRECTION('',(0.734385107701325,0.,0.678733020845836));
#30367=DIRECTION('',(0.69001582900495,0.,0.723794277210459));
#30368=DIRECTION('',(0.639367837579431,0.,0.768901013309907));
#30369=DIRECTION('',(0.580576328166246,0.,0.814205826049531));
#30370=DIRECTION('',(0.510236429716899,0.,0.860034177105626));
#30371=DIRECTION('',(-0.10256186711098,0.,-0.99472662747848));
#30372=DIRECTION('',(0.998680786707765,0.,-0.0513486734079864));
#30373=DIRECTION('',(0.998680786707765,0.,0.0513486734079863));
#30374=DIRECTION('',(-0.102561867110979,0.,0.99472662747848));
#30375=DIRECTION('',(0.5102364297169,0.,-0.860034177105626));
#30376=DIRECTION('',(0.580576328166246,0.,-0.814205826049532));
#30377=DIRECTION('',(0.639367837579431,0.,-0.768901013309908));
#30378=DIRECTION('',(0.69001582900495,0.,-0.723794277210459));
#30379=DIRECTION('',(0.734385107701325,0.,-0.678733020845836));
#30380=DIRECTION('',(0.77362520182667,0.,-0.63364347001973));
#30381=DIRECTION('',(0.971437971490766,0.,0.237293631490407));
#30382=DIRECTION('',(0.967816336590582,0.,0.251657582099936));
#30383=DIRECTION('',(0.963982324735007,0.,0.265966309141763));
#30384=DIRECTION('',(0.959936777257023,0.,0.280216672718455));
#30385=DIRECTION('',(0.353157342779899,0.,0.935563942892543));
#30386=DIRECTION('',(0.296629649007407,0.,0.954992592290507));
#30387=DIRECTION('',(0.235674098326432,0.,0.97183214568053));
#30388=DIRECTION('',(0.169258283051555,0.,0.985571729311692));
#30389=DIRECTION('',(0.0956909360031021,0.,0.99541109335131));
#30390=DIRECTION('',(0.0118606215182939,0.,0.999929660354767));
#30391=DIRECTION('',(0.408542131361567,0.,-0.912739462772673));
#30392=DIRECTION('',(0.890557268264349,0.,0.45487113773193));
#30393=DIRECTION('',(0.839208594856358,0.,0.543809648975832));
#30394=DIRECTION('',(-0.586184496116913,0.,0.810177595661693));
#30395=DIRECTION('',(0.87189479862393,0.,-0.489693230637852));
#30396=DIRECTION('',(0.909896762052632,0.,-0.41483476518505));
#30397=DIRECTION('',(0.938159296361463,0.,-0.346203891732262));
#30398=DIRECTION('',(0.95946837553689,0.,-0.2818163166756));
#30399=DIRECTION('',(0.975362669853239,0.,-0.220607484589173));
#30400=DIRECTION('',(0.986800812799624,0.,-0.161938741065875));
#30401=DIRECTION('',(0.722643145766637,0.,0.691221298772324));
#30402=DIRECTION('',(0.712324742635063,0.,0.701850027448807));
#30403=DIRECTION('',(0.701850027448807,0.,0.712324742635063));
#30404=DIRECTION('',(0.691221298772316,0.,0.722643145766645));
#30405=DIRECTION('',(-0.161938741065862,0.,0.986800812799627));
#30406=DIRECTION('',(-0.220607484589184,0.,0.975362669853236));
#30407=DIRECTION('',(-0.281816316675577,0.,0.959468375536896));
#30408=DIRECTION('',(-0.346203891732263,0.,0.938159296361463));
#30409=DIRECTION('',(-0.414834765185061,0.,0.909896762052627));
#30410=DIRECTION('',(-0.48969323063785,0.,0.871894798623931));
#30411=DIRECTION('',(0.810177595661695,0.,-0.58618449611691));
#30412=DIRECTION('',(0.543809648975831,0.,0.839208594856359));
#30413=DIRECTION('',(0.454871137731933,0.,0.890557268264347));
#30414=DIRECTION('',(-0.912739462772673,0.,0.408542131361568));
#30415=DIRECTION('',(0.999929660354767,0.,0.0118606215182843));
#30416=DIRECTION('',(0.99541109335131,0.,0.0956909360030991));
#30417=DIRECTION('',(0.98557172931169,0.,0.169258283051569));
#30418=DIRECTION('',(0.971832145680534,0.,0.235674098326418));
#30419=DIRECTION('',(0.954992592290506,0.,0.29662964900741));
#30420=DIRECTION('',(0.935563942892542,0.,0.3531573427799));
#30421=DIRECTION('',(0.280216672718472,0.,0.959936777257017));
#30422=DIRECTION('',(0.265966309141757,0.,0.963982324735009));
#30423=DIRECTION('',(0.251657582099955,0.,0.967816336590577));
#30424=DIRECTION('',(0.237293631490361,0.,0.971437971490778));
#30425=DIRECTION('',(-0.633643470019724,0.,0.773625201826675));
#30426=DIRECTION('',(-0.678733020845831,0.,0.734385107701329));
#30427=DIRECTION('',(-0.723794277210464,0.,0.690015829004945));
#30428=DIRECTION('',(-0.768901013309907,0.,0.639367837579431));
#30429=DIRECTION('',(-0.814205826049529,0.,0.580576328166249));
#30430=DIRECTION('',(-0.860034177105627,0.,0.510236429716898));
#30431=DIRECTION('',(0.99472662747848,0.,-0.102561867110979));
#30432=DIRECTION('',(0.0513486734079878,0.,0.998680786707765));
#30433=DIRECTION('',(-0.0513486734079865,0.,0.998680786707765));
#30434=DIRECTION('',(-0.99472662747848,0.,-0.102561867110979));
#30435=DIRECTION('',(0.860034177105627,0.,0.510236429716898));
#30436=DIRECTION('',(0.814205826049526,0.,0.580576328166254));
#30437=DIRECTION('',(0.768901013309911,0.,0.639367837579427));
#30438=DIRECTION('',(0.723794277210468,0.,0.690015829004942));
#30439=DIRECTION('',(0.678733020845828,0.,0.734385107701332));
#30440=DIRECTION('',(0.633643470019728,0.,0.773625201826672));
#30441=DIRECTION('',(-0.237293631490364,0.,0.971437971490777));
#30442=DIRECTION('',(-0.251657582099965,0.,0.967816336590574));
#30443=DIRECTION('',(-0.265966309141746,0.,0.963982324735012));
#30444=DIRECTION('',(-0.280216672718472,0.,0.959936777257017));
#30445=DIRECTION('',(-0.93556394289254,0.,0.353157342779907));
#30446=DIRECTION('',(-0.954992592290506,0.,0.29662964900741));
#30447=DIRECTION('',(-0.971832145680531,0.,0.235674098326429));
#30448=DIRECTION('',(-0.985571729311693,0.,0.169258283051549));
#30449=DIRECTION('',(-0.995411093351309,0.,0.0956909360031064));
#30450=DIRECTION('',(-0.999929660354767,0.,0.0118606215182996));
#30451=DIRECTION('',(0.912739462772674,0.,0.408542131361566));
#30452=DIRECTION('',(-0.454871137731933,0.,0.890557268264347));
#30453=DIRECTION('center_axis',(0.,-1.,0.));
#30454=DIRECTION('ref_axis',(0.,0.,1.));
#30455=DIRECTION('center_axis',(0.871894798623931,0.,-0.48969323063785));
#30456=DIRECTION('ref_axis',(-0.48969323063785,0.,-0.871894798623931));
#30457=DIRECTION('',(0.,1.,0.));
#30458=DIRECTION('',(-0.451594888615274,-0.386714295024759,-0.80406101173982));
#30459=DIRECTION('',(-0.48969323063785,0.,-0.871894798623931));
#30460=DIRECTION('',(0.,1.,0.));
#30461=DIRECTION('center_axis',(0.817918893329126,0.,-0.575333541465521));
#30462=DIRECTION('ref_axis',(-0.575333541465521,0.,-0.817918893329126));
#30463=DIRECTION('',(0.,1.,0.));
#30464=DIRECTION('',(-0.547096153529848,-0.309436927624307,-0.777775408852244));
#30465=DIRECTION('center_axis',(0.0725221917253267,-0.70710678118655,-0.703377943716856));
#30466=DIRECTION('ref_axis',(-0.99472662747848,0.,-0.102561867110979));
#30467=DIRECTION('',(0.793123151629957,-0.386714295024742,0.470539818051651));
#30468=DIRECTION('',(-0.0363329527197043,-0.706639907076674,0.706639907076678));
#30469=DIRECTION('',(0.99472662747848,0.,0.102561867110979));
#30470=DIRECTION('',(0.945142170174665,-0.176491388068499,0.274876459696312));
#30471=DIRECTION('',(0.862686871695709,-0.309436927624321,0.400025185739962));
#30472=DIRECTION('center_axis',(0.510236429716898,0.,-0.860034177105627));
#30473=DIRECTION('ref_axis',(-0.860034177105627,0.,-0.510236429716898));
#30474=DIRECTION('',(0.,1.,0.));
#30475=DIRECTION('',(-0.793123151629957,-0.386714295024742,-0.470539818051651));
#30476=DIRECTION('',(-0.860034177105627,0.,-0.510236429716898));
#30477=DIRECTION('',(0.,1.,0.));
#30478=DIRECTION('center_axis',(0.420671769125535,0.,-0.907212909222963));
#30479=DIRECTION('ref_axis',(-0.907212909222963,0.,-0.420671769125535));
#30480=DIRECTION('',(0.,1.,0.));
#30481=DIRECTION('',(-0.862686871695709,-0.309436927624321,-0.400025185739962));
#30482=DIRECTION('center_axis',(-0.28888291148617,-0.707106781186549,-0.645404263583122));
#30483=DIRECTION('ref_axis',(-0.912739462772673,0.,0.408542131361568));
#30484=DIRECTION('',(0.922134706666949,-0.386714295024736,0.0109378601098506));
#30485=DIRECTION('',(0.321854693488575,-0.706639907076675,0.630134587216131));
#30486=DIRECTION('',(0.912739462772673,0.,-0.408542131361568));
#30487=DIRECTION('',(0.955955359407371,-0.176491388068498,-0.234521088087999));
#30488=DIRECTION('',(0.94712133926979,-0.309436927624331,-0.0849114628434474));
#30489=DIRECTION('center_axis',(0.0118606215182843,0.,-0.999929660354767));
#30490=DIRECTION('ref_axis',(-0.999929660354767,0.,-0.0118606215182843));
#30491=DIRECTION('',(0.,1.,0.));
#30492=DIRECTION('',(-0.922134706666949,-0.386714295024736,-0.0109378601098506));
#30493=DIRECTION('',(-0.999929660354767,0.,-0.0118606215182843));
#30494=DIRECTION('',(0.,1.,0.));
#30495=DIRECTION('center_axis',(-0.0892940158938145,0.,-0.996005310591041));
#30496=DIRECTION('ref_axis',(-0.996005310591041,0.,0.0892940158938145));
#30497=DIRECTION('',(0.,1.,0.));
#30498=DIRECTION('',(-0.94712133926979,-0.309436927624331,0.0849114628434474));
#30499=DIRECTION('center_axis',(-0.572882071857796,-0.707106781186548,-0.414495032230688));
#30500=DIRECTION('ref_axis',(-0.586184496116912,0.,0.810177595661693));
#30501=DIRECTION('',(0.804061011739819,-0.386714295024756,-0.451594888615276));
#30502=DIRECTION('',(0.593801634496424,-0.706639907076676,0.384785213588103));
#30503=DIRECTION('',(0.586184496116913,0.,-0.810177595661693));
#30504=DIRECTION('',(0.710621082086668,-0.176491388068499,-0.681078899711059));
#30505=DIRECTION('',(0.777775408852244,-0.309436927624306,-0.547096153529848));
#30506=DIRECTION('center_axis',(-0.489693230637852,0.,-0.87189479862393));
#30507=DIRECTION('ref_axis',(-0.87189479862393,0.,0.489693230637852));
#30508=DIRECTION('',(0.,1.,0.));
#30509=DIRECTION('',(-0.804061011739819,-0.386714295024756,0.451594888615276));
#30510=DIRECTION('',(-0.87189479862393,0.,0.489693230637852));
#30511=DIRECTION('',(0.,1.,0.));
#30512=DIRECTION('center_axis',(-0.575333541465521,0.,-0.817918893329126));
#30513=DIRECTION('ref_axis',(-0.817918893329126,0.,0.57533354146552));
#30514=DIRECTION('',(0.,1.,0.));
#30515=DIRECTION('',(-0.777775408852244,-0.309436927624306,0.547096153529848));
#30516=DIRECTION('center_axis',(-0.703377943716856,-0.707106781186549,-0.0725221917253265));
#30517=DIRECTION('ref_axis',(-0.102561867110979,0.,0.99472662747848));
#30518=DIRECTION('',(0.470539818051652,-0.386714295024744,-0.793123151629956));
#30519=DIRECTION('',(0.706639907076678,-0.706639907076675,0.0363329527197041));
#30520=DIRECTION('',(0.102561867110979,0.,-0.99472662747848));
#30521=DIRECTION('',(0.274876459696313,-0.176491388068501,-0.945142170174665));
#30522=DIRECTION('',(0.400025185739966,-0.309436927624327,-0.862686871695706));
#30523=DIRECTION('center_axis',(-0.860034177105626,0.,-0.5102364297169));
#30524=DIRECTION('ref_axis',(-0.5102364297169,0.,0.860034177105626));
#30525=DIRECTION('',(0.,1.,0.));
#30526=DIRECTION('',(-0.470539818051652,-0.386714295024744,0.793123151629956));
#30527=DIRECTION('',(-0.5102364297169,0.,0.860034177105626));
#30528=DIRECTION('',(0.,1.,0.));
#30529=DIRECTION('center_axis',(-0.907212909222961,0.,-0.42067176912554));
#30530=DIRECTION('ref_axis',(-0.42067176912554,0.,0.907212909222961));
#30531=DIRECTION('',(0.,1.,0.));
#30532=DIRECTION('',(-0.400025185739966,-0.309436927624327,0.862686871695706));
#30533=DIRECTION('center_axis',(-0.645404263583122,-0.707106781186549,0.288882911486169));
#30534=DIRECTION('ref_axis',(0.408542131361568,0.,0.912739462772673));
#30535=DIRECTION('',(0.0109378601098593,-0.386714295024742,-0.922134706666946));
#30536=DIRECTION('',(0.630134587216131,-0.706639907076675,-0.321854693488576));
#30537=DIRECTION('',(-0.408542131361568,0.,-0.912739462772673));
#30538=DIRECTION('',(-0.234521088087998,-0.176491388068499,-0.955955359407371));
#30539=DIRECTION('',(-0.0849114628434554,-0.309436927624324,-0.947121339269791));
#30540=DIRECTION('center_axis',(-0.999929660354767,0.,-0.0118606215182939));
#30541=DIRECTION('ref_axis',(-0.0118606215182939,0.,0.999929660354767));
#30542=DIRECTION('',(0.,1.,0.));
#30543=DIRECTION('',(-0.0109378601098593,-0.386714295024742,0.922134706666946));
#30544=DIRECTION('',(-0.0118606215182939,0.,0.999929660354767));
#30545=DIRECTION('',(0.,1.,0.));
#30546=DIRECTION('center_axis',(-0.99600531059104,0.,0.0892940158938226));
#30547=DIRECTION('ref_axis',(0.0892940158938226,0.,0.99600531059104));
#30548=DIRECTION('',(0.,1.,0.));
#30549=DIRECTION('',(0.0849114628434554,-0.309436927624324,0.947121339269791));
#30550=DIRECTION('center_axis',(-0.414495032230688,-0.707106781186549,0.572882071857795));
#30551=DIRECTION('ref_axis',(0.810177595661692,0.,0.586184496116913));
#30552=DIRECTION('',(-0.451594888615301,-0.386714295024736,-0.804061011739815));
#30553=DIRECTION('',(0.384785213588103,-0.706639907076675,-0.593801634496425));
#30554=DIRECTION('',(-0.810177595661692,0.,-0.586184496116913));
#30555=DIRECTION('',(-0.681078899711046,-0.176491388068513,-0.710621082086678));
#30556=DIRECTION('',(-0.547096153529855,-0.309436927624298,-0.777775408852242));
#30557=DIRECTION('center_axis',(-0.871894798623917,0.,0.489693230637875));
#30558=DIRECTION('ref_axis',(0.489693230637875,0.,0.871894798623917));
#30559=DIRECTION('',(0.,1.,0.));
#30560=DIRECTION('',(0.451594888615301,-0.386714295024736,0.804061011739815));
#30561=DIRECTION('',(0.489693230637875,0.,0.871894798623917));
#30562=DIRECTION('',(0.,1.,0.));
#30563=DIRECTION('center_axis',(-0.817918893329121,0.,0.575333541465527));
#30564=DIRECTION('ref_axis',(0.575333541465527,0.,0.817918893329121));
#30565=DIRECTION('',(0.,1.,0.));
#30566=DIRECTION('',(0.547096153529855,-0.309436927624298,0.777775408852242));
#30567=DIRECTION('center_axis',(-0.0725221917253267,-0.70710678118655,0.703377943716856));
#30568=DIRECTION('ref_axis',(0.99472662747848,0.,0.102561867110979));
#30569=DIRECTION('',(-0.793123151629962,-0.386714295024737,-0.470539818051647));
#30570=DIRECTION('',(0.0363329527197052,-0.706639907076674,-0.706639907076678));
#30571=DIRECTION('',(-0.99472662747848,0.,-0.102561867110979));
#30572=DIRECTION('',(-0.945142170174656,-0.17649138806852,-0.274876459696332));
#30573=DIRECTION('',(-0.862686871695723,-0.309436927624304,-0.400025185739946));
#30574=DIRECTION('center_axis',(-0.510236429716893,0.,0.86003417710563));
#30575=DIRECTION('ref_axis',(0.86003417710563,0.,0.510236429716893));
#30576=DIRECTION('',(0.,1.,0.));
#30577=DIRECTION('',(0.793123151629962,-0.386714295024737,0.470539818051647));
#30578=DIRECTION('',(0.86003417710563,0.,0.510236429716893));
#30579=DIRECTION('',(0.,1.,0.));
#30580=DIRECTION('center_axis',(-0.420671769125515,0.,0.907212909222972));
#30581=DIRECTION('ref_axis',(0.907212909222972,0.,0.420671769125515));
#30582=DIRECTION('',(0.,1.,0.));
#30583=DIRECTION('',(0.862686871695723,-0.309436927624304,0.400025185739946));
#30584=DIRECTION('center_axis',(0.28888291148617,-0.707106781186549,0.645404263583122));
#30585=DIRECTION('ref_axis',(0.912739462772673,0.,-0.408542131361568));
#30586=DIRECTION('',(-0.922134706666946,-0.386714295024741,-0.0109378601098575));
#30587=DIRECTION('',(-0.321854693488575,-0.706639907076675,-0.630134587216131));
#30588=DIRECTION('',(-0.912739462772673,0.,0.408542131361568));
#30589=DIRECTION('',(-0.955955359407372,-0.176491388068506,0.23452108808799));
#30590=DIRECTION('',(-0.947121339269795,-0.309436927624305,0.0849114628434785));
#30591=DIRECTION('center_axis',(-0.0118606215182919,0.,0.999929660354767));
#30592=DIRECTION('ref_axis',(0.999929660354767,0.,0.0118606215182919));
#30593=DIRECTION('',(0.,1.,0.));
#30594=DIRECTION('',(0.922134706666946,-0.386714295024741,0.0109378601098575));
#30595=DIRECTION('',(0.999929660354767,0.,0.0118606215182919));
#30596=DIRECTION('',(0.,1.,0.));
#30597=DIRECTION('center_axis',(0.0892940158938463,0.,0.996005310591038));
#30598=DIRECTION('ref_axis',(0.996005310591038,0.,-0.0892940158938463));
#30599=DIRECTION('',(0.,1.,0.));
#30600=DIRECTION('',(0.947121339269795,-0.309436927624305,-0.0849114628434785));
#30601=DIRECTION('center_axis',(0.572882071857795,-0.707106781186549,0.414495032230687));
#30602=DIRECTION('ref_axis',(0.586184496116912,0.,-0.810177595661693));
#30603=DIRECTION('',(-0.804061011739815,-0.386714295024737,0.4515948886153));
#30604=DIRECTION('',(-0.593801634496426,-0.706639907076675,-0.384785213588102));
#30605=DIRECTION('',(-0.586184496116912,0.,0.810177595661693));
#30606=DIRECTION('',(-0.710621082086674,-0.176491388068508,0.681078899711051));
#30607=DIRECTION('',(-0.777775408852245,-0.309436927624309,0.547096153529844));
#30608=DIRECTION('center_axis',(0.489693230637874,0.,0.871894798623917));
#30609=DIRECTION('ref_axis',(0.871894798623918,0.,-0.489693230637874));
#30610=DIRECTION('',(0.,1.,0.));
#30611=DIRECTION('',(0.804061011739815,-0.386714295024737,-0.4515948886153));
#30612=DIRECTION('',(0.871894798623918,0.,-0.489693230637874));
#30613=DIRECTION('',(0.,1.,0.));
#30614=DIRECTION('center_axis',(0.575333541465517,0.,0.817918893329128));
#30615=DIRECTION('ref_axis',(0.817918893329128,0.,-0.575333541465517));
#30616=DIRECTION('',(0.,1.,0.));
#30617=DIRECTION('',(0.777775408852245,-0.309436927624309,-0.547096153529844));
#30618=DIRECTION('center_axis',(0.703377943716856,-0.707106781186549,0.0725221917253273));
#30619=DIRECTION('ref_axis',(0.10256186711098,0.,-0.99472662747848));
#30620=DIRECTION('',(-0.470539818051651,-0.386714295024741,0.793123151629958));
#30621=DIRECTION('',(-0.706639907076678,-0.706639907076675,-0.0363329527197062));
#30622=DIRECTION('',(-0.10256186711098,0.,0.99472662747848));
#30623=DIRECTION('',(-0.27487645969631,-0.176491388068497,0.945142170174666));
#30624=DIRECTION('',(-0.400025185739954,-0.309436927624312,0.862686871695717));
#30625=DIRECTION('center_axis',(0.860034177105628,0.,0.510236429716897));
#30626=DIRECTION('ref_axis',(0.510236429716897,0.,-0.860034177105627));
#30627=DIRECTION('',(0.,1.,0.));
#30628=DIRECTION('',(0.470539818051651,-0.386714295024741,-0.793123151629958));
#30629=DIRECTION('',(0.510236429716897,0.,-0.860034177105627));
#30630=DIRECTION('',(0.,1.,0.));
#30631=DIRECTION('center_axis',(0.907212909222968,0.,0.420671769125525));
#30632=DIRECTION('ref_axis',(0.420671769125525,0.,-0.907212909222968));
#30633=DIRECTION('',(0.,1.,0.));
#30634=DIRECTION('',(0.400025185739954,-0.309436927624312,-0.862686871695717));
#30635=DIRECTION('center_axis',(0.645404263583121,-0.70710678118655,-0.288882911486169));
#30636=DIRECTION('ref_axis',(-0.408542131361568,0.,-0.912739462772673));
#30637=DIRECTION('',(-0.0109378601098576,-0.38671429502474,0.922134706666947));
#30638=DIRECTION('',(-0.630134587216131,-0.706639907076674,0.321854693488576));
#30639=DIRECTION('',(0.408542131361568,0.,0.912739462772673));
#30640=DIRECTION('',(0.234521088088,-0.176491388068496,0.955955359407371));
#30641=DIRECTION('',(0.0849114628434721,-0.30943692762431,0.947121339269795));
#30642=DIRECTION('center_axis',(0.999929660354767,0.,0.011860621518292));
#30643=DIRECTION('ref_axis',(0.011860621518292,0.,-0.999929660354767));
#30644=DIRECTION('',(0.,1.,0.));
#30645=DIRECTION('',(0.0109378601098576,-0.38671429502474,-0.922134706666947));
#30646=DIRECTION('',(0.011860621518292,0.,-0.999929660354767));
#30647=DIRECTION('',(0.,1.,0.));
#30648=DIRECTION('center_axis',(0.996005310591038,0.,-0.0892940158938398));
#30649=DIRECTION('ref_axis',(-0.0892940158938398,0.,-0.996005310591038));
#30650=DIRECTION('',(0.,1.,0.));
#30651=DIRECTION('',(-0.0849114628434721,-0.30943692762431,-0.947121339269795));
#30652=DIRECTION('center_axis',(-0.572882071857796,-0.707106781186548,0.414495032230686));
#30653=DIRECTION('ref_axis',(0.58618449611691,0.,0.810177595661694));
#30654=DIRECTION('',(-0.710621082086669,0.176491388068502,-0.681078899711058));
#30655=DIRECTION('',(-0.58618449611691,0.,-0.810177595661694));
#30656=DIRECTION('',(-0.593801634496424,0.706639907076676,0.384785213588103));
#30657=DIRECTION('',(-0.804061011739819,0.386714295024758,-0.451594888615275));
#30658=DIRECTION('',(-0.777775408852245,0.309436927624312,-0.547096153529842));
#30659=DIRECTION('center_axis',(-0.810177595661694,0.,0.58618449611691));
#30660=DIRECTION('ref_axis',(0.58618449611691,0.,0.810177595661694));
#30661=DIRECTION('',(0.,1.,0.));
#30662=DIRECTION('',(0.58618449611691,0.,0.810177595661694));
#30663=DIRECTION('',(0.,1.,0.));
#30664=DIRECTION('center_axis',(-0.691940859832156,0.,0.721954185869669));
#30665=DIRECTION('ref_axis',(0.721954185869669,0.,0.691940859832156));
#30666=DIRECTION('',(0.,1.,0.));
#30667=DIRECTION('',(0.710621082086669,0.176491388068502,0.681078899711058));
#30668=DIRECTION('center_axis',(-0.288882911486168,-0.707106781186549,0.645404263583123));
#30669=DIRECTION('ref_axis',(0.912739462772674,0.,0.408542131361566));
#30670=DIRECTION('',(-0.955955359407371,0.176491388068495,-0.234521088088));
#30671=DIRECTION('',(-0.912739462772674,0.,-0.408542131361566));
#30672=DIRECTION('',(-0.321854693488574,0.706639907076675,0.630134587216131));
#30673=DIRECTION('',(-0.922134706666944,0.386714295024745,0.0109378601098646));
#30674=DIRECTION('',(-0.947121339269793,0.309436927624317,-0.0849114628434623));
#30675=DIRECTION('center_axis',(-0.408542131361566,0.,0.912739462772674));
#30676=DIRECTION('ref_axis',(0.912739462772674,0.,0.408542131361566));
#30677=DIRECTION('',(0.,1.,0.));
#30678=DIRECTION('',(0.912739462772674,0.,0.408542131361566));
#30679=DIRECTION('',(0.,1.,0.));
#30680=DIRECTION('center_axis',(-0.238261269596264,0.,0.971201095247723));
#30681=DIRECTION('ref_axis',(0.971201095247723,0.,0.238261269596264));
#30682=DIRECTION('',(0.,1.,0.));
#30683=DIRECTION('',(0.955955359407371,0.176491388068495,0.234521088088));
#30684=DIRECTION('center_axis',(0.0725221917253267,-0.70710678118655,0.703377943716856));
#30685=DIRECTION('ref_axis',(0.99472662747848,0.,-0.102561867110979));
#30686=DIRECTION('',(-0.945142170174669,0.176491388068491,0.274876459696304));
#30687=DIRECTION('',(-0.99472662747848,0.,0.102561867110979));
#30688=DIRECTION('',(0.0363329527197052,0.706639907076674,0.706639907076678));
#30689=DIRECTION('',(-0.793123151629957,0.386714295024742,0.470539818051651));
#30690=DIRECTION('',(-0.8626868716957,0.309436927624333,0.400025185739973));
#30691=DIRECTION('center_axis',(0.102561867110979,0.,0.99472662747848));
#30692=DIRECTION('ref_axis',(0.99472662747848,0.,-0.102561867110979));
#30693=DIRECTION('',(0.,1.,0.));
#30694=DIRECTION('',(0.99472662747848,0.,-0.102561867110979));
#30695=DIRECTION('',(0.,1.,0.));
#30696=DIRECTION('center_axis',(0.279260235415558,0.,0.960215455465932));
#30697=DIRECTION('ref_axis',(0.960215455465932,0.,-0.279260235415558));
#30698=DIRECTION('',(0.,1.,0.));
#30699=DIRECTION('',(0.945142170174669,0.176491388068491,-0.274876459696304));
#30700=DIRECTION('center_axis',(0.414495032230686,-0.707106781186548,0.572882071857796));
#30701=DIRECTION('ref_axis',(0.810177595661695,0.,-0.58618449611691));
#30702=DIRECTION('',(-0.681078899711047,0.176491388068514,0.710621082086676));
#30703=DIRECTION('',(-0.810177595661695,0.,0.58618449611691));
#30704=DIRECTION('',(0.384785213588102,0.706639907076676,0.593801634496425));
#30705=DIRECTION('',(-0.451594888615274,0.386714295024759,0.804061011739819));
#30706=DIRECTION('',(-0.547096153529855,0.309436927624302,0.777775408852241));
#30707=DIRECTION('center_axis',(0.58618449611691,0.,0.810177595661695));
#30708=DIRECTION('ref_axis',(0.810177595661695,0.,-0.58618449611691));
#30709=DIRECTION('',(0.,1.,0.));
#30710=DIRECTION('',(0.810177595661695,0.,-0.58618449611691));
#30711=DIRECTION('',(0.,1.,0.));
#30712=DIRECTION('center_axis',(0.721954185869678,0.,0.691940859832147));
#30713=DIRECTION('ref_axis',(0.691940859832147,0.,-0.721954185869678));
#30714=DIRECTION('',(0.,1.,0.));
#30715=DIRECTION('',(0.681078899711047,0.176491388068514,-0.710621082086676));
#30716=DIRECTION('center_axis',(0.64540426358312,-0.707106781186551,0.288882911486168));
#30717=DIRECTION('ref_axis',(0.408542131361567,0.,-0.912739462772673));
#30718=DIRECTION('',(-0.234521088087998,0.176491388068497,0.955955359407371));
#30719=DIRECTION('',(-0.408542131361567,0.,0.912739462772673));
#30720=DIRECTION('',(0.630134587216134,0.706639907076673,0.321854693488573));
#30721=DIRECTION('',(0.0109378601098593,0.38671429502474,0.922134706666947));
#30722=DIRECTION('',(-0.0849114628434554,0.309436927624323,0.947121339269792));
#30723=DIRECTION('center_axis',(0.912739462772673,0.,0.408542131361567));
#30724=DIRECTION('ref_axis',(0.408542131361567,0.,-0.912739462772673));
#30725=DIRECTION('',(0.,1.,0.));
#30726=DIRECTION('',(0.408542131361567,0.,-0.912739462772673));
#30727=DIRECTION('',(0.,1.,0.));
#30728=DIRECTION('center_axis',(0.971201095247723,0.,0.238261269596262));
#30729=DIRECTION('ref_axis',(0.238261269596262,0.,-0.971201095247723));
#30730=DIRECTION('',(0.,1.,0.));
#30731=DIRECTION('',(0.234521088087998,0.176491388068497,-0.955955359407371));
#30732=DIRECTION('center_axis',(0.703377943716856,-0.707106781186549,-0.0725221917253273));
#30733=DIRECTION('ref_axis',(-0.10256186711098,0.,-0.99472662747848));
#30734=DIRECTION('',(0.27487645969631,0.176491388068496,0.945142170174667));
#30735=DIRECTION('',(0.10256186711098,0.,0.99472662747848));
#30736=DIRECTION('',(0.706639907076678,0.706639907076675,-0.0363329527197042));
#30737=DIRECTION('',(0.470539818051652,0.386714295024743,0.793123151629956));
#30738=DIRECTION('',(0.400025185739966,0.309436927624326,0.862686871695706));
#30739=DIRECTION('center_axis',(0.99472662747848,0.,-0.10256186711098));
#30740=DIRECTION('ref_axis',(-0.10256186711098,0.,-0.99472662747848));
#30741=DIRECTION('',(0.,1.,0.));
#30742=DIRECTION('',(-0.10256186711098,0.,-0.99472662747848));
#30743=DIRECTION('',(0.,1.,0.));
#30744=DIRECTION('center_axis',(0.96021545546593,0.,-0.279260235415564));
#30745=DIRECTION('ref_axis',(-0.279260235415564,0.,-0.96021545546593));
#30746=DIRECTION('',(0.,1.,0.));
#30747=DIRECTION('',(-0.27487645969631,0.176491388068496,-0.945142170174667));
#30748=DIRECTION('center_axis',(0.572882071857795,-0.707106781186549,-0.414495032230686));
#30749=DIRECTION('ref_axis',(-0.586184496116911,0.,-0.810177595661694));
#30750=DIRECTION('',(0.710621082086668,0.1764913880685,0.681078899711059));
#30751=DIRECTION('',(0.586184496116911,0.,0.810177595661694));
#30752=DIRECTION('',(0.593801634496425,0.706639907076675,-0.384785213588104));
#30753=DIRECTION('',(0.804061011739822,0.386714295024766,0.451594888615263));
#30754=DIRECTION('',(0.777775408852243,0.309436927624306,0.547096153529849));
#30755=DIRECTION('center_axis',(0.810177595661694,0.,-0.586184496116911));
#30756=DIRECTION('ref_axis',(-0.586184496116911,0.,-0.810177595661694));
#30757=DIRECTION('',(0.,1.,0.));
#30758=DIRECTION('',(-0.586184496116911,0.,-0.810177595661694));
#30759=DIRECTION('',(0.,1.,0.));
#30760=DIRECTION('center_axis',(0.691940859832157,0.,-0.721954185869668));
#30761=DIRECTION('ref_axis',(-0.721954185869668,0.,-0.691940859832157));
#30762=DIRECTION('',(0.,1.,0.));
#30763=DIRECTION('',(-0.710621082086668,0.1764913880685,-0.681078899711059));
#30764=DIRECTION('center_axis',(0.28888291148617,-0.707106781186549,-0.645404263583122));
#30765=DIRECTION('ref_axis',(-0.912739462772673,0.,-0.408542131361568));
#30766=DIRECTION('',(0.955955359407372,0.176491388068506,0.234521088087991));
#30767=DIRECTION('',(0.912739462772673,0.,0.408542131361568));
#30768=DIRECTION('',(0.321854693488575,0.706639907076675,-0.630134587216131));
#30769=DIRECTION('',(0.922134706666946,0.386714295024741,-0.0109378601098576));
#30770=DIRECTION('',(0.947121339269794,0.309436927624312,0.0849114628434706));
#30771=DIRECTION('center_axis',(0.408542131361568,0.,-0.912739462772673));
#30772=DIRECTION('ref_axis',(-0.912739462772673,0.,-0.408542131361568));
#30773=DIRECTION('',(0.,1.,0.));
#30774=DIRECTION('',(-0.912739462772673,0.,-0.408542131361568));
#30775=DIRECTION('',(0.,1.,0.));
#30776=DIRECTION('center_axis',(0.238261269596255,0.,-0.971201095247725));
#30777=DIRECTION('ref_axis',(-0.971201095247725,0.,-0.238261269596255));
#30778=DIRECTION('',(0.,1.,0.));
#30779=DIRECTION('',(-0.955955359407372,0.176491388068506,-0.234521088087991));
#30780=DIRECTION('center_axis',(-0.0725221917253267,-0.70710678118655,-0.703377943716856));
#30781=DIRECTION('ref_axis',(-0.99472662747848,0.,0.102561867110979));
#30782=DIRECTION('',(0.945142170174659,0.176491388068513,-0.274876459696325));
#30783=DIRECTION('',(0.99472662747848,0.,-0.102561867110979));
#30784=DIRECTION('',(-0.0363329527197052,0.706639907076674,-0.706639907076678));
#30785=DIRECTION('',(0.793123151629962,0.386714295024737,-0.470539818051647));
#30786=DIRECTION('',(0.862686871695719,0.30943692762431,-0.400025185739951));
#30787=DIRECTION('center_axis',(-0.102561867110979,0.,-0.99472662747848));
#30788=DIRECTION('ref_axis',(-0.99472662747848,0.,0.102561867110979));
#30789=DIRECTION('',(0.,1.,0.));
#30790=DIRECTION('',(-0.99472662747848,0.,0.102561867110979));
#30791=DIRECTION('',(0.,1.,0.));
#30792=DIRECTION('center_axis',(-0.279260235415581,0.,-0.960215455465925));
#30793=DIRECTION('ref_axis',(-0.960215455465925,0.,0.279260235415581));
#30794=DIRECTION('',(0.,1.,0.));
#30795=DIRECTION('',(-0.945142170174659,0.176491388068513,0.274876459696325));
#30796=DIRECTION('center_axis',(-0.414495032230688,-0.707106781186549,-0.572882071857795));
#30797=DIRECTION('ref_axis',(-0.810177595661692,0.,0.586184496116913));
#30798=DIRECTION('',(0.681078899711057,0.1764913880685,-0.71062108208667));
#30799=DIRECTION('',(0.810177595661692,0.,-0.586184496116913));
#30800=DIRECTION('',(-0.384785213588103,0.706639907076675,-0.593801634496425));
#30801=DIRECTION('',(0.451594888615294,0.386714295024742,-0.804061011739817));
#30802=DIRECTION('',(0.547096153529844,0.309436927624308,-0.777775408852246));
#30803=DIRECTION('center_axis',(-0.586184496116913,0.,-0.810177595661692));
#30804=DIRECTION('ref_axis',(-0.810177595661692,0.,0.586184496116913));
#30805=DIRECTION('',(0.,1.,0.));
#30806=DIRECTION('',(-0.810177595661692,0.,0.586184496116913));
#30807=DIRECTION('',(0.,1.,0.));
#30808=DIRECTION('center_axis',(-0.72195418586967,0.,-0.691940859832155));
#30809=DIRECTION('ref_axis',(-0.691940859832155,0.,0.72195418586967));
#30810=DIRECTION('',(0.,1.,0.));
#30811=DIRECTION('',(-0.681078899711057,0.1764913880685,0.71062108208667));
#30812=DIRECTION('center_axis',(-0.645404263583121,-0.70710678118655,-0.288882911486169));
#30813=DIRECTION('ref_axis',(-0.408542131361568,0.,0.912739462772673));
#30814=DIRECTION('',(0.234521088087999,0.176491388068497,-0.955955359407371));
#30815=DIRECTION('',(0.408542131361568,0.,-0.912739462772673));
#30816=DIRECTION('',(-0.630134587216131,0.706639907076674,-0.321854693488577));
#30817=DIRECTION('',(-0.0109378601098559,0.386714295024739,-0.922134706666947));
#30818=DIRECTION('',(0.0849114628434702,0.309436927624312,-0.947121339269794));
#30819=DIRECTION('center_axis',(-0.912739462772673,0.,-0.408542131361568));
#30820=DIRECTION('ref_axis',(-0.408542131361568,0.,0.912739462772673));
#30821=DIRECTION('',(0.,1.,0.));
#30822=DIRECTION('',(-0.408542131361568,0.,0.912739462772673));
#30823=DIRECTION('',(0.,1.,0.));
#30824=DIRECTION('center_axis',(-0.971201095247723,0.,-0.238261269596264));
#30825=DIRECTION('ref_axis',(-0.238261269596264,0.,0.971201095247723));
#30826=DIRECTION('',(0.,1.,0.));
#30827=DIRECTION('',(-0.234521088087999,0.176491388068497,0.955955359407371));
#30828=DIRECTION('center_axis',(-0.703377943716856,-0.707106781186549,0.0725221917253272));
#30829=DIRECTION('ref_axis',(0.10256186711098,0.,0.99472662747848));
#30830=DIRECTION('',(-0.27487645969631,0.176491388068497,-0.945142170174666));
#30831=DIRECTION('',(-0.10256186711098,0.,-0.99472662747848));
#30832=DIRECTION('',(-0.706639907076678,0.706639907076675,0.0363329527197063));
#30833=DIRECTION('',(-0.47053981805165,0.386714295024741,-0.793123151629958));
#30834=DIRECTION('',(-0.400025185739953,0.309436927624312,-0.862686871695717));
#30835=DIRECTION('center_axis',(-0.99472662747848,0.,0.10256186711098));
#30836=DIRECTION('ref_axis',(0.10256186711098,0.,0.99472662747848));
#30837=DIRECTION('',(0.,1.,0.));
#30838=DIRECTION('',(0.10256186711098,0.,0.99472662747848));
#30839=DIRECTION('',(0.,1.,0.));
#30840=DIRECTION('center_axis',(-0.96021545546593,0.,0.279260235415565));
#30841=DIRECTION('ref_axis',(0.279260235415565,0.,0.96021545546593));
#30842=DIRECTION('',(0.,1.,0.));
#30843=DIRECTION('',(0.27487645969631,0.176491388068497,0.945142170174666));
#30844=DIRECTION('center_axis',(0.645404263583121,0.70710678118655,-0.288882911486169));
#30845=DIRECTION('ref_axis',(-0.408542131361568,0.,-0.912739462772673));
#30846=DIRECTION('',(-0.234521088088,-0.176491388068496,-0.955955359407371));
#30847=DIRECTION('',(-0.408542131361568,0.,-0.912739462772673));
#30848=DIRECTION('',(0.630134587216131,-0.706639907076674,-0.321854693488576));
#30849=DIRECTION('',(0.408542131361568,0.,0.912739462772673));
#30850=DIRECTION('center_axis',(0.,1.,0.));
#30851=DIRECTION('ref_axis',(0.,0.,1.));
#30852=DIRECTION('',(0.890557268264346,0.,-0.454871137731935));
#30853=DIRECTION('',(0.839208594856358,0.,-0.543809648975832));
#30854=DIRECTION('',(-0.58618449611691,0.,-0.810177595661694));
#30855=DIRECTION('',(0.87189479862393,0.,0.489693230637852));
#30856=DIRECTION('',(0.909896762052626,0.,0.414834765185062));
#30857=DIRECTION('',(0.938159296361463,0.,0.346203891732262));
#30858=DIRECTION('',(0.959468375536896,0.,0.28181631667558));
#30859=DIRECTION('',(0.975362669853236,0.,0.220607484589183));
#30860=DIRECTION('',(0.986800812799626,0.,0.161938741065865));
#30861=DIRECTION('',(0.722643145766653,0.,-0.691221298772308));
#30862=DIRECTION('',(0.712324742635051,0.,-0.701850027448819));
#30863=DIRECTION('',(0.701850027448819,0.,-0.712324742635051));
#30864=DIRECTION('',(0.691221298772304,0.,-0.722643145766656));
#30865=DIRECTION('',(-0.161938741065869,0.,-0.986800812799626));
#30866=DIRECTION('',(-0.220607484589178,0.,-0.975362669853237));
#30867=DIRECTION('',(-0.281816316675586,0.,-0.959468375536894));
#30868=DIRECTION('',(-0.346203891732264,0.,-0.938159296361463));
#30869=DIRECTION('',(-0.414834765185058,0.,-0.909896762052629));
#30870=DIRECTION('',(0.810177595661694,0.,0.586184496116911));
#30871=DIRECTION('',(0.54380964897583,0.,-0.839208594856359));
#30872=DIRECTION('',(0.454871137731933,0.,-0.890557268264347));
#30873=DIRECTION('',(-0.912739462772674,0.,-0.408542131361566));
#30874=DIRECTION('',(0.999929660354767,0.,-0.0118606215182996));
#30875=DIRECTION('',(0.995411093351309,0.,-0.0956909360031064));
#30876=DIRECTION('',(0.985571729311693,0.,-0.169258283051549));
#30877=DIRECTION('',(0.971832145680531,0.,-0.235674098326429));
#30878=DIRECTION('',(0.954992592290506,0.,-0.29662964900741));
#30879=DIRECTION('',(0.93556394289254,0.,-0.353157342779907));
#30880=DIRECTION('',(0.280216672718472,0.,-0.959936777257017));
#30881=DIRECTION('',(0.265966309141746,0.,-0.963982324735012));
#30882=DIRECTION('',(0.251657582099965,0.,-0.967816336590574));
#30883=DIRECTION('',(0.237293631490364,0.,-0.971437971490777));
#30884=DIRECTION('',(-0.633643470019728,0.,-0.773625201826672));
#30885=DIRECTION('',(-0.678733020845828,0.,-0.734385107701332));
#30886=DIRECTION('',(-0.723794277210468,0.,-0.690015829004942));
#30887=DIRECTION('',(-0.768901013309911,0.,-0.639367837579427));
#30888=DIRECTION('',(-0.814205826049526,0.,-0.580576328166254));
#30889=DIRECTION('',(0.99472662747848,0.,0.102561867110979));
#30890=DIRECTION('',(0.0513486734079865,0.,-0.998680786707765));
#30891=DIRECTION('',(-0.0513486734079878,0.,-0.998680786707765));
#30892=DIRECTION('',(-0.99472662747848,0.,0.102561867110979));
#30893=DIRECTION('',(0.860034177105627,0.,-0.510236429716898));
#30894=DIRECTION('',(0.814205826049529,0.,-0.580576328166249));
#30895=DIRECTION('',(0.768901013309907,0.,-0.639367837579431));
#30896=DIRECTION('',(0.723794277210464,0.,-0.690015829004945));
#30897=DIRECTION('',(0.678733020845831,0.,-0.734385107701329));
#30898=DIRECTION('',(0.633643470019724,0.,-0.773625201826675));
#30899=DIRECTION('',(-0.237293631490361,0.,-0.971437971490778));
#30900=DIRECTION('',(-0.251657582099955,0.,-0.967816336590577));
#30901=DIRECTION('',(-0.265966309141757,0.,-0.963982324735009));
#30902=DIRECTION('',(-0.280216672718472,0.,-0.959936777257017));
#30903=DIRECTION('',(-0.935563942892542,0.,-0.3531573427799));
#30904=DIRECTION('',(-0.954992592290506,0.,-0.29662964900741));
#30905=DIRECTION('',(-0.971832145680534,0.,-0.235674098326418));
#30906=DIRECTION('',(-0.98557172931169,0.,-0.169258283051569));
#30907=DIRECTION('',(-0.99541109335131,0.,-0.0956909360030991));
#30908=DIRECTION('',(0.912739462772673,0.,-0.408542131361568));
#30909=DIRECTION('',(-0.454871137731933,0.,-0.890557268264347));
#30910=DIRECTION('',(-0.543809648975831,0.,-0.839208594856359));
#30911=DIRECTION('',(-0.810177595661695,0.,0.58618449611691));
#30912=DIRECTION('',(0.48969323063785,0.,-0.871894798623931));
#30913=DIRECTION('',(0.414834765185061,0.,-0.909896762052627));
#30914=DIRECTION('',(0.346203891732263,0.,-0.938159296361463));
#30915=DIRECTION('',(0.281816316675577,0.,-0.959468375536896));
#30916=DIRECTION('',(0.220607484589184,0.,-0.975362669853236));
#30917=DIRECTION('',(0.161938741065862,0.,-0.986800812799627));
#30918=DIRECTION('',(-0.691221298772316,0.,-0.722643145766645));
#30919=DIRECTION('',(-0.701850027448807,0.,-0.712324742635063));
#30920=DIRECTION('',(-0.712324742635063,0.,-0.701850027448807));
#30921=DIRECTION('',(-0.722643145766637,0.,-0.691221298772324));
#30922=DIRECTION('',(-0.986800812799624,0.,0.161938741065875));
#30923=DIRECTION('',(-0.975362669853239,0.,0.220607484589173));
#30924=DIRECTION('',(-0.95946837553689,0.,0.2818163166756));
#30925=DIRECTION('',(-0.938159296361463,0.,0.346203891732262));
#30926=DIRECTION('',(-0.909896762052632,0.,0.41483476518505));
#30927=DIRECTION('',(0.586184496116913,0.,-0.810177595661693));
#30928=DIRECTION('',(-0.839208594856358,0.,-0.543809648975832));
#30929=DIRECTION('',(-0.890557268264349,0.,-0.45487113773193));
#30930=DIRECTION('',(-0.408542131361567,0.,0.912739462772673));
#30931=DIRECTION('',(-0.0118606215182939,0.,-0.999929660354767));
#30932=DIRECTION('',(-0.0956909360031021,0.,-0.99541109335131));
#30933=DIRECTION('',(-0.169258283051555,0.,-0.985571729311692));
#30934=DIRECTION('',(-0.235674098326432,0.,-0.97183214568053));
#30935=DIRECTION('',(-0.296629649007407,0.,-0.954992592290507));
#30936=DIRECTION('',(-0.353157342779899,0.,-0.935563942892543));
#30937=DIRECTION('',(-0.959936777257023,0.,-0.280216672718455));
#30938=DIRECTION('',(-0.963982324735007,0.,-0.265966309141763));
#30939=DIRECTION('',(-0.967816336590582,0.,-0.251657582099936));
#30940=DIRECTION('',(-0.971437971490766,0.,-0.237293631490407));
#30941=DIRECTION('',(-0.77362520182667,0.,0.63364347001973));
#30942=DIRECTION('',(-0.734385107701325,0.,0.678733020845836));
#30943=DIRECTION('',(-0.69001582900495,0.,0.723794277210459));
#30944=DIRECTION('',(-0.639367837579431,0.,0.768901013309908));
#30945=DIRECTION('',(-0.580576328166246,0.,0.814205826049532));
#30946=DIRECTION('',(0.102561867110979,0.,-0.99472662747848));
#30947=DIRECTION('',(-0.998680786707765,0.,-0.0513486734079863));
#30948=DIRECTION('',(-0.998680786707765,0.,0.0513486734079864));
#30949=DIRECTION('',(0.10256186711098,0.,0.99472662747848));
#30950=DIRECTION('',(-0.510236429716899,0.,-0.860034177105626));
#30951=DIRECTION('',(-0.580576328166246,0.,-0.814205826049531));
#30952=DIRECTION('',(-0.639367837579431,0.,-0.768901013309907));
#30953=DIRECTION('',(-0.69001582900495,0.,-0.723794277210459));
#30954=DIRECTION('',(-0.734385107701325,0.,-0.678733020845836));
#30955=DIRECTION('',(-0.773625201826676,0.,-0.633643470019722));
#30956=DIRECTION('',(-0.971437971490773,0.,0.237293631490379));
#30957=DIRECTION('',(-0.967816336590582,0.,0.251657582099936));
#30958=DIRECTION('',(-0.963982324735007,0.,0.265966309141761));
#30959=DIRECTION('',(-0.959936777257014,0.,0.280216672718486));
#30960=DIRECTION('',(-0.3531573427799,0.,0.935563942892542));
#30961=DIRECTION('',(-0.296629649007409,0.,0.954992592290506));
#30962=DIRECTION('',(-0.235674098326432,0.,0.97183214568053));
#30963=DIRECTION('',(-0.169258283051555,0.,0.985571729311692));
#30964=DIRECTION('',(-0.0956909360031021,0.,0.99541109335131));
#30965=DIRECTION('',(-0.408542131361568,0.,-0.912739462772673));
#30966=DIRECTION('',(-0.890557268264346,0.,0.454871137731935));
#30967=DIRECTION('',(-0.839208594856358,0.,0.543809648975832));
#30968=DIRECTION('',(0.586184496116911,0.,0.810177595661694));
#30969=DIRECTION('',(-0.871894798623937,0.,-0.48969323063784));
#30970=DIRECTION('',(-0.909896762052627,0.,-0.414834765185061));
#30971=DIRECTION('',(-0.938159296361463,0.,-0.346203891732263));
#30972=DIRECTION('',(-0.959468375536898,0.,-0.281816316675571));
#30973=DIRECTION('',(-0.975362669853233,0.,-0.2206074845892));
#30974=DIRECTION('',(-0.986800812799626,0.,-0.161938741065863));
#30975=DIRECTION('',(-0.722643145766668,0.,0.691221298772292));
#30976=DIRECTION('',(-0.71232474263504,0.,0.701850027448831));
#30977=DIRECTION('',(-0.701850027448823,0.,0.712324742635048));
#30978=DIRECTION('',(-0.691221298772293,0.,0.722643145766667));
#30979=DIRECTION('',(0.161938741065865,0.,0.986800812799626));
#30980=DIRECTION('',(0.22060748458919,0.,0.975362669853235));
#30981=DIRECTION('',(0.281816316675564,0.,0.9594683755369));
#30982=DIRECTION('',(0.346203891732269,0.,0.938159296361461));
#30983=DIRECTION('',(0.414834765185046,0.,0.909896762052634));
#30984=DIRECTION('',(-0.810177595661692,0.,-0.586184496116913));
#30985=DIRECTION('',(-0.543809648975832,0.,0.839208594856358));
#30986=DIRECTION('',(-0.454871137731933,0.,0.890557268264347));
#30987=DIRECTION('',(0.912739462772673,0.,0.408542131361568));
#30988=DIRECTION('',(-0.999929660354767,0.,0.011860621518292));
#30989=DIRECTION('',(-0.99541109335131,0.,0.0956909360031057));
#30990=DIRECTION('',(-0.985571729311695,0.,0.169258283051542));
#30991=DIRECTION('',(-0.971832145680524,0.,0.235674098326456));
#30992=DIRECTION('',(-0.95499259229051,0.,0.296629649007398));
#30993=DIRECTION('',(-0.935563942892542,0.,0.3531573427799));
#30994=DIRECTION('',(-0.280216672718478,0.,0.959936777257016));
#30995=DIRECTION('',(-0.265966309141754,0.,0.963982324735009));
#30996=DIRECTION('',(-0.251657582099958,0.,0.967816336590576));
#30997=DIRECTION('',(-0.237293631490357,0.,0.971437971490779));
#30998=DIRECTION('',(0.63364347001972,0.,0.773625201826678));
#30999=DIRECTION('',(0.678733020845838,0.,0.734385107701322));
#31000=DIRECTION('',(0.723794277210454,0.,0.690015829004956));
#31001=DIRECTION('',(0.768901013309911,0.,0.639367837579427));
#31002=DIRECTION('',(0.814205826049522,0.,0.580576328166259));
#31003=DIRECTION('',(-0.99472662747848,0.,-0.102561867110979));
#31004=DIRECTION('',(-0.0513486734079878,0.,0.998680786707765));
#31005=DIRECTION('',(0.0513486734079878,0.,0.998680786707765));
#31006=DIRECTION('',(0.99472662747848,0.,-0.102561867110979));
#31007=DIRECTION('',(-0.86003417710563,0.,0.510236429716893));
#31008=DIRECTION('',(-0.814205826049519,0.,0.580576328166263));
#31009=DIRECTION('',(-0.768901013309918,0.,0.639367837579419));
#31010=DIRECTION('',(-0.723794277210445,0.,0.690015829004965));
#31011=DIRECTION('',(-0.678733020845843,0.,0.734385107701318));
#31012=DIRECTION('',(-0.633643470019724,0.,0.773625201826675));
#31013=DIRECTION('',(0.237293631490368,0.,0.971437971490776));
#31014=DIRECTION('',(0.251657582099958,0.,0.967816336590576));
#31015=DIRECTION('',(0.265966309141754,0.,0.963982324735009));
#31016=DIRECTION('',(0.280216672718464,0.,0.95993677725702));
#31017=DIRECTION('',(0.93556394289254,0.,0.353157342779906));
#31018=DIRECTION('',(0.954992592290512,0.,0.296629649007392));
#31019=DIRECTION('',(0.971832145680526,0.,0.235674098326448));
#31020=DIRECTION('',(0.985571729311693,0.,0.169258283051549));
#31021=DIRECTION('',(0.995411093351309,0.,0.0956909360031137));
#31022=DIRECTION('',(-0.912739462772673,0.,0.408542131361568));
#31023=DIRECTION('',(0.454871137731934,0.,0.890557268264347));
#31024=DIRECTION('',(0.543809648975831,0.,0.839208594856358));
#31025=DIRECTION('',(0.810177595661692,0.,-0.586184496116913));
#31026=DIRECTION('',(-0.489693230637868,0.,0.871894798623921));
#31027=DIRECTION('',(-0.414834765185049,0.,0.909896762052633));
#31028=DIRECTION('',(-0.346203891732272,0.,0.93815929636146));
#31029=DIRECTION('',(-0.281816316675565,0.,0.9594683755369));
#31030=DIRECTION('',(-0.220607484589187,0.,0.975362669853235));
#31031=DIRECTION('',(-0.161938741065865,0.,0.986800812799626));
#31032=DIRECTION('',(0.691221298772312,0.,0.722643145766649));
#31033=DIRECTION('',(0.701850027448815,0.,0.712324742635055));
#31034=DIRECTION('',(0.712324742635051,0.,0.701850027448819));
#31035=DIRECTION('',(0.722643145766652,0.,0.691221298772308));
#31036=DIRECTION('',(0.986800812799626,0.,-0.161938741065868));
#31037=DIRECTION('',(0.975362669853236,0.,-0.220607484589184));
#31038=DIRECTION('',(0.9594683755369,0.,-0.281816316675565));
#31039=DIRECTION('',(0.938159296361459,0.,-0.346203891732275));
#31040=DIRECTION('',(0.909896762052635,0.,-0.414834765185043));
#31041=DIRECTION('',(-0.586184496116912,0.,0.810177595661693));
#31042=DIRECTION('',(0.839208594856359,0.,0.54380964897583));
#31043=DIRECTION('',(0.890557268264346,0.,0.454871137731935));
#31044=DIRECTION('',(0.408542131361568,0.,-0.912739462772673));
#31045=DIRECTION('',(0.0118606215182901,0.,0.999929660354767));
#31046=DIRECTION('',(0.0956909360031101,0.,0.995411093351309));
#31047=DIRECTION('',(0.169258283051554,0.,0.985571729311692));
#31048=DIRECTION('',(0.235674098326447,0.,0.971832145680527));
#31049=DIRECTION('',(0.296629649007399,0.,0.954992592290509));
#31050=DIRECTION('',(0.353157342779898,0.,0.935563942892543));
#31051=DIRECTION('',(0.959936777257018,0.,0.28021667271847));
#31052=DIRECTION('',(0.963982324735007,0.,0.265966309141762));
#31053=DIRECTION('',(0.967816336590576,0.,0.251657582099957));
#31054=DIRECTION('',(0.971437971490777,0.,0.237293631490364));
#31055=DIRECTION('',(0.773625201826672,0.,-0.633643470019727));
#31056=DIRECTION('',(0.734385107701324,0.,-0.678733020845836));
#31057=DIRECTION('',(0.690015829004958,0.,-0.723794277210452));
#31058=DIRECTION('',(0.639367837579427,0.,-0.768901013309911));
#31059=DIRECTION('',(0.580576328166257,0.,-0.814205826049523));
#31060=DIRECTION('',(-0.10256186711098,0.,0.99472662747848));
#31061=DIRECTION('',(0.998680786707765,0.,0.0513486734079893));
#31062=DIRECTION('',(0.998680786707765,0.,-0.0513486734079894));
#31063=DIRECTION('',(-0.10256186711098,0.,-0.99472662747848));
#31064=DIRECTION('',(0.510236429716897,0.,0.860034177105627));
#31065=DIRECTION('',(0.580576328166257,0.,0.814205826049523));
#31066=DIRECTION('',(0.639367837579427,0.,0.768901013309911));
#31067=DIRECTION('',(0.690015829004958,0.,0.723794277210452));
#31068=DIRECTION('',(0.734385107701324,0.,0.678733020845837));
#31069=DIRECTION('',(0.773625201826672,0.,0.633643470019727));
#31070=DIRECTION('',(0.971437971490777,0.,-0.237293631490364));
#31071=DIRECTION('',(0.967816336590576,0.,-0.251657582099957));
#31072=DIRECTION('',(0.963982324735009,0.,-0.265966309141754));
#31073=DIRECTION('',(0.959936777257016,0.,-0.280216672718478));
#31074=DIRECTION('',(0.353157342779898,0.,-0.935563942892543));
#31075=DIRECTION('',(0.296629649007403,0.,-0.954992592290508));
#31076=DIRECTION('',(0.235674098326445,0.,-0.971832145680527));
#31077=DIRECTION('',(0.169258283051556,0.,-0.985571729311692));
#31078=DIRECTION('',(0.0956909360031075,0.,-0.995411093351309));
#31079=DIRECTION('center_axis',(0.,1.,0.));
#31080=DIRECTION('ref_axis',(0.,0.,1.));
#31081=DIRECTION('center_axis',(-0.703377943716856,0.707106781186549,0.0725221917253272));
#31082=DIRECTION('ref_axis',(0.10256186711098,0.,0.99472662747848));
#31083=DIRECTION('',(0.47053981805165,0.386714295024741,0.793123151629958));
#31084=DIRECTION('',(0.706639907076678,0.706639907076675,-0.0363329527197063));
#31085=DIRECTION('',(0.400025185739953,0.309436927624312,0.862686871695717));
#31086=DIRECTION('center_axis',(0.703377943716856,0.707106781186549,0.0725221917253273));
#31087=DIRECTION('ref_axis',(0.10256186711098,0.,-0.99472662747848));
#31088=DIRECTION('',(0.27487645969631,-0.176491388068497,-0.945142170174666));
#31089=DIRECTION('',(0.10256186711098,0.,-0.99472662747848));
#31090=DIRECTION('',(0.706639907076678,-0.706639907076675,0.0363329527197062));
#31091=DIRECTION('center_axis',(-0.645404263583121,0.70710678118655,-0.288882911486169));
#31092=DIRECTION('ref_axis',(-0.408542131361568,0.,0.912739462772673));
#31093=DIRECTION('',(0.0109378601098559,0.386714295024739,0.922134706666947));
#31094=DIRECTION('',(0.630134587216131,0.706639907076674,0.321854693488577));
#31095=DIRECTION('',(-0.0849114628434702,0.309436927624312,0.947121339269794));
#31096=DIRECTION('center_axis',(0.572882071857795,0.707106781186549,0.414495032230687));
#31097=DIRECTION('ref_axis',(0.586184496116912,0.,-0.810177595661693));
#31098=DIRECTION('',(0.710621082086674,-0.176491388068508,-0.681078899711051));
#31099=DIRECTION('',(0.586184496116912,0.,-0.810177595661693));
#31100=DIRECTION('',(0.593801634496426,-0.706639907076675,0.384785213588102));
#31101=DIRECTION('center_axis',(-0.414495032230688,0.707106781186549,-0.572882071857795));
#31102=DIRECTION('ref_axis',(-0.810177595661692,0.,0.586184496116913));
#31103=DIRECTION('',(-0.451594888615294,0.386714295024742,0.804061011739817));
#31104=DIRECTION('',(0.384785213588103,0.706639907076675,0.593801634496425));
#31105=DIRECTION('',(-0.547096153529844,0.309436927624308,0.777775408852246));
#31106=DIRECTION('center_axis',(0.28888291148617,0.707106781186549,0.645404263583122));
#31107=DIRECTION('ref_axis',(0.912739462772673,0.,-0.408542131361568));
#31108=DIRECTION('',(0.955955359407372,-0.176491388068506,-0.23452108808799));
#31109=DIRECTION('',(0.912739462772673,0.,-0.408542131361568));
#31110=DIRECTION('',(0.321854693488575,-0.706639907076675,0.630134587216131));
#31111=DIRECTION('center_axis',(-0.0725221917253267,0.70710678118655,-0.703377943716856));
#31112=DIRECTION('ref_axis',(-0.99472662747848,0.,0.102561867110979));
#31113=DIRECTION('',(-0.793123151629962,0.386714295024737,0.470539818051647));
#31114=DIRECTION('',(0.0363329527197052,0.706639907076674,0.706639907076678));
#31115=DIRECTION('',(-0.862686871695719,0.30943692762431,0.400025185739951));
#31116=DIRECTION('center_axis',(-0.0725221917253267,0.70710678118655,0.703377943716856));
#31117=DIRECTION('ref_axis',(0.99472662747848,0.,0.102561867110979));
#31118=DIRECTION('',(0.945142170174656,-0.17649138806852,0.274876459696332));
#31119=DIRECTION('',(0.99472662747848,0.,0.102561867110979));
#31120=DIRECTION('',(-0.0363329527197052,-0.706639907076674,0.706639907076678));
#31121=DIRECTION('center_axis',(0.28888291148617,0.707106781186549,-0.645404263583122));
#31122=DIRECTION('ref_axis',(-0.912739462772673,0.,-0.408542131361568));
#31123=DIRECTION('',(-0.922134706666946,0.386714295024741,0.0109378601098576));
#31124=DIRECTION('',(-0.321854693488575,0.706639907076675,0.630134587216131));
#31125=DIRECTION('',(-0.947121339269794,0.309436927624312,-0.0849114628434706));
#31126=DIRECTION('center_axis',(-0.414495032230688,0.707106781186549,0.572882071857795));
#31127=DIRECTION('ref_axis',(0.810177595661692,0.,0.586184496116913));
#31128=DIRECTION('',(0.681078899711046,-0.176491388068513,0.710621082086678));
#31129=DIRECTION('',(0.810177595661692,0.,0.586184496116913));
#31130=DIRECTION('',(-0.384785213588103,-0.706639907076675,0.593801634496425));
#31131=DIRECTION('center_axis',(0.572882071857795,0.707106781186549,-0.414495032230686));
#31132=DIRECTION('ref_axis',(-0.586184496116911,0.,-0.810177595661694));
#31133=DIRECTION('',(-0.804061011739822,0.386714295024766,-0.451594888615263));
#31134=DIRECTION('',(-0.593801634496425,0.706639907076675,0.384785213588104));
#31135=DIRECTION('',(-0.777775408852243,0.309436927624306,-0.547096153529849));
#31136=DIRECTION('center_axis',(-0.645404263583122,0.707106781186549,0.288882911486169));
#31137=DIRECTION('ref_axis',(0.408542131361568,0.,0.912739462772673));
#31138=DIRECTION('',(0.234521088087998,-0.176491388068499,0.955955359407371));
#31139=DIRECTION('',(0.408542131361568,0.,0.912739462772673));
#31140=DIRECTION('',(-0.630134587216131,-0.706639907076675,0.321854693488576));
#31141=DIRECTION('center_axis',(0.703377943716856,0.707106781186549,-0.0725221917253273));
#31142=DIRECTION('ref_axis',(-0.10256186711098,0.,-0.99472662747848));
#31143=DIRECTION('',(-0.470539818051652,0.386714295024743,-0.793123151629956));
#31144=DIRECTION('',(-0.706639907076678,0.706639907076675,0.0363329527197042));
#31145=DIRECTION('',(-0.400025185739966,0.309436927624326,-0.862686871695706));
#31146=DIRECTION('center_axis',(-0.703377943716856,0.707106781186549,-0.0725221917253265));
#31147=DIRECTION('ref_axis',(-0.102561867110979,0.,0.99472662747848));
#31148=DIRECTION('',(-0.274876459696313,-0.176491388068501,0.945142170174665));
#31149=DIRECTION('',(-0.102561867110979,0.,0.99472662747848));
#31150=DIRECTION('',(-0.706639907076678,-0.706639907076675,-0.0363329527197041));
#31151=DIRECTION('center_axis',(0.64540426358312,0.707106781186551,0.288882911486168));
#31152=DIRECTION('ref_axis',(0.408542131361567,0.,-0.912739462772673));
#31153=DIRECTION('',(-0.0109378601098593,0.38671429502474,-0.922134706666947));
#31154=DIRECTION('',(-0.630134587216134,0.706639907076673,-0.321854693488573));
#31155=DIRECTION('',(0.0849114628434554,0.309436927624323,-0.947121339269792));
#31156=DIRECTION('center_axis',(-0.572882071857796,0.707106781186548,-0.414495032230688));
#31157=DIRECTION('ref_axis',(-0.586184496116912,0.,0.810177595661693));
#31158=DIRECTION('',(-0.710621082086668,-0.176491388068499,0.681078899711059));
#31159=DIRECTION('',(-0.586184496116913,0.,0.810177595661693));
#31160=DIRECTION('',(-0.593801634496424,-0.706639907076676,-0.384785213588103));
#31161=DIRECTION('center_axis',(0.414495032230686,0.707106781186548,0.572882071857796));
#31162=DIRECTION('ref_axis',(0.810177595661695,0.,-0.58618449611691));
#31163=DIRECTION('',(0.451594888615274,0.386714295024759,-0.804061011739819));
#31164=DIRECTION('',(-0.384785213588102,0.706639907076676,-0.593801634496425));
#31165=DIRECTION('',(0.547096153529855,0.309436927624302,-0.777775408852241));
#31166=DIRECTION('center_axis',(-0.28888291148617,0.707106781186549,-0.645404263583122));
#31167=DIRECTION('ref_axis',(-0.912739462772673,0.,0.408542131361568));
#31168=DIRECTION('',(-0.955955359407371,-0.176491388068498,0.234521088087999));
#31169=DIRECTION('',(-0.912739462772673,0.,0.408542131361568));
#31170=DIRECTION('',(-0.321854693488575,-0.706639907076675,-0.630134587216131));
#31171=DIRECTION('center_axis',(0.0725221917253267,0.70710678118655,0.703377943716856));
#31172=DIRECTION('ref_axis',(0.99472662747848,0.,-0.102561867110979));
#31173=DIRECTION('',(0.793123151629957,0.386714295024742,-0.470539818051651));
#31174=DIRECTION('',(-0.0363329527197052,0.706639907076674,-0.706639907076678));
#31175=DIRECTION('',(0.8626868716957,0.309436927624333,-0.400025185739973));
#31176=DIRECTION('center_axis',(0.0725221917253267,0.70710678118655,-0.703377943716856));
#31177=DIRECTION('ref_axis',(-0.99472662747848,0.,-0.102561867110979));
#31178=DIRECTION('',(-0.945142170174665,-0.176491388068499,-0.274876459696312));
#31179=DIRECTION('',(-0.99472662747848,0.,-0.102561867110979));
#31180=DIRECTION('',(0.0363329527197043,-0.706639907076674,-0.706639907076678));
#31181=DIRECTION('center_axis',(-0.288882911486168,0.707106781186549,0.645404263583123));
#31182=DIRECTION('ref_axis',(0.912739462772674,0.,0.408542131361566));
#31183=DIRECTION('',(0.922134706666944,0.386714295024745,-0.0109378601098646));
#31184=DIRECTION('',(0.321854693488574,0.706639907076675,-0.630134587216131));
#31185=DIRECTION('',(0.947121339269793,0.309436927624317,0.0849114628434623));
#31186=DIRECTION('center_axis',(0.414495032230687,0.707106781186548,-0.572882071857796));
#31187=DIRECTION('ref_axis',(-0.810177595661694,0.,-0.586184496116911));
#31188=DIRECTION('',(-0.681078899711059,-0.1764913880685,-0.710621082086668));
#31189=DIRECTION('',(-0.810177595661694,0.,-0.586184496116911));
#31190=DIRECTION('',(0.384785213588102,-0.706639907076676,-0.593801634496425));
#31191=DIRECTION('center_axis',(-0.572882071857796,0.707106781186548,0.414495032230686));
#31192=DIRECTION('ref_axis',(0.58618449611691,0.,0.810177595661694));
#31193=DIRECTION('',(0.804061011739819,0.386714295024758,0.451594888615275));
#31194=DIRECTION('',(0.593801634496424,0.706639907076676,-0.384785213588103));
#31195=DIRECTION('',(0.777775408852245,0.309436927624312,0.547096153529842));
#31196=DIRECTION('center_axis',(0.454871137731935,0.,0.890557268264346));
#31197=DIRECTION('ref_axis',(0.890557268264346,0.,-0.454871137731935));
#31198=DIRECTION('',(0.,1.,0.));
#31199=DIRECTION('',(0.,1.,0.));
#31200=DIRECTION('center_axis',(0.912739462772673,0.,-0.408542131361568));
#31201=DIRECTION('ref_axis',(-0.408542131361568,0.,-0.912739462772673));
#31202=DIRECTION('',(0.,1.,0.));
#31203=DIRECTION('center_axis',(0.971201095247723,0.,-0.238261269596264));
#31204=DIRECTION('ref_axis',(-0.238261269596264,0.,-0.971201095247723));
#31205=DIRECTION('center_axis',(0.995411093351309,0.,0.0956909360031075));
#31206=DIRECTION('ref_axis',(0.0956909360031075,0.,-0.995411093351309));
#31207=DIRECTION('',(0.,1.,0.));
#31208=DIRECTION('center_axis',(0.985571729311692,0.,0.169258283051556));
#31209=DIRECTION('ref_axis',(0.169258283051556,0.,-0.985571729311692));
#31210=DIRECTION('',(0.,1.,0.));
#31211=DIRECTION('center_axis',(0.971832145680527,0.,0.235674098326445));
#31212=DIRECTION('ref_axis',(0.235674098326445,0.,-0.971832145680527));
#31213=DIRECTION('',(0.,1.,0.));
#31214=DIRECTION('center_axis',(0.954992592290508,0.,0.296629649007403));
#31215=DIRECTION('ref_axis',(0.296629649007403,0.,-0.954992592290508));
#31216=DIRECTION('',(0.,1.,0.));
#31217=DIRECTION('center_axis',(0.935563942892543,0.,0.353157342779898));
#31218=DIRECTION('ref_axis',(0.353157342779898,0.,-0.935563942892543));
#31219=DIRECTION('',(0.,1.,0.));
#31220=DIRECTION('center_axis',(0.280216672718478,0.,0.959936777257016));
#31221=DIRECTION('ref_axis',(0.959936777257016,0.,-0.280216672718478));
#31222=DIRECTION('',(0.,1.,0.));
#31223=DIRECTION('center_axis',(0.265966309141754,0.,0.963982324735009));
#31224=DIRECTION('ref_axis',(0.963982324735009,0.,-0.265966309141754));
#31225=DIRECTION('',(0.,1.,0.));
#31226=DIRECTION('center_axis',(0.251657582099958,0.,0.967816336590576));
#31227=DIRECTION('ref_axis',(0.967816336590576,0.,-0.251657582099958));
#31228=DIRECTION('',(0.,1.,0.));
#31229=DIRECTION('center_axis',(0.237293631490364,0.,0.971437971490777));
#31230=DIRECTION('ref_axis',(0.971437971490777,0.,-0.237293631490364));
#31231=DIRECTION('',(0.,1.,0.));
#31232=DIRECTION('center_axis',(-0.633643470019727,0.,0.773625201826672));
#31233=DIRECTION('ref_axis',(0.773625201826672,0.,0.633643470019727));
#31234=DIRECTION('',(0.,1.,0.));
#31235=DIRECTION('center_axis',(-0.678733020845837,0.,0.734385107701324));
#31236=DIRECTION('ref_axis',(0.734385107701324,0.,0.678733020845837));
#31237=DIRECTION('',(0.,1.,0.));
#31238=DIRECTION('center_axis',(-0.723794277210452,0.,0.690015829004958));
#31239=DIRECTION('ref_axis',(0.690015829004958,0.,0.723794277210452));
#31240=DIRECTION('',(0.,1.,0.));
#31241=DIRECTION('center_axis',(-0.768901013309911,0.,0.639367837579427));
#31242=DIRECTION('ref_axis',(0.639367837579427,0.,0.768901013309911));
#31243=DIRECTION('',(0.,1.,0.));
#31244=DIRECTION('center_axis',(-0.814205826049523,0.,0.580576328166257));
#31245=DIRECTION('ref_axis',(0.580576328166257,0.,0.814205826049523));
#31246=DIRECTION('',(0.,1.,0.));
#31247=DIRECTION('center_axis',(-0.860034177105628,0.,0.510236429716897));
#31248=DIRECTION('ref_axis',(0.510236429716897,0.,0.860034177105627));
#31249=DIRECTION('',(0.,1.,0.));
#31250=DIRECTION('center_axis',(-0.907212909222968,0.,0.420671769125524));
#31251=DIRECTION('ref_axis',(0.420671769125524,0.,0.907212909222968));
#31252=DIRECTION('center_axis',(0.0513486734079894,0.,0.998680786707765));
#31253=DIRECTION('ref_axis',(0.998680786707765,0.,-0.0513486734079894));
#31254=DIRECTION('',(0.,1.,0.));
#31255=DIRECTION('center_axis',(-0.0513486734079893,0.,0.998680786707765));
#31256=DIRECTION('ref_axis',(0.998680786707765,0.,0.0513486734079893));
#31257=DIRECTION('',(0.,1.,0.));
#31258=DIRECTION('center_axis',(0.99472662747848,0.,0.10256186711098));
#31259=DIRECTION('ref_axis',(0.10256186711098,0.,-0.99472662747848));
#31260=DIRECTION('',(0.,1.,0.));
#31261=DIRECTION('center_axis',(0.96021545546593,0.,0.279260235415565));
#31262=DIRECTION('ref_axis',(0.279260235415565,0.,-0.96021545546593));
#31263=DIRECTION('center_axis',(0.814205826049523,0.,0.580576328166257));
#31264=DIRECTION('ref_axis',(0.580576328166257,0.,-0.814205826049523));
#31265=DIRECTION('',(0.,1.,0.));
#31266=DIRECTION('center_axis',(0.768901013309911,0.,0.639367837579427));
#31267=DIRECTION('ref_axis',(0.639367837579427,0.,-0.768901013309911));
#31268=DIRECTION('',(0.,1.,0.));
#31269=DIRECTION('center_axis',(0.723794277210452,0.,0.690015829004958));
#31270=DIRECTION('ref_axis',(0.690015829004958,0.,-0.723794277210452));
#31271=DIRECTION('',(0.,1.,0.));
#31272=DIRECTION('center_axis',(0.678733020845836,0.,0.734385107701324));
#31273=DIRECTION('ref_axis',(0.734385107701324,0.,-0.678733020845836));
#31274=DIRECTION('',(0.,1.,0.));
#31275=DIRECTION('center_axis',(0.633643470019727,0.,0.773625201826672));
#31276=DIRECTION('ref_axis',(0.773625201826672,0.,-0.633643470019727));
#31277=DIRECTION('',(0.,1.,0.));
#31278=DIRECTION('center_axis',(-0.237293631490364,0.,0.971437971490777));
#31279=DIRECTION('ref_axis',(0.971437971490777,0.,0.237293631490364));
#31280=DIRECTION('',(0.,1.,0.));
#31281=DIRECTION('center_axis',(-0.251657582099957,0.,0.967816336590576));
#31282=DIRECTION('ref_axis',(0.967816336590576,0.,0.251657582099957));
#31283=DIRECTION('',(0.,1.,0.));
#31284=DIRECTION('center_axis',(-0.265966309141762,0.,0.963982324735007));
#31285=DIRECTION('ref_axis',(0.963982324735007,0.,0.265966309141762));
#31286=DIRECTION('',(0.,1.,0.));
#31287=DIRECTION('center_axis',(-0.28021667271847,0.,0.959936777257018));
#31288=DIRECTION('ref_axis',(0.959936777257018,0.,0.28021667271847));
#31289=DIRECTION('',(0.,1.,0.));
#31290=DIRECTION('center_axis',(-0.935563942892543,0.,0.353157342779898));
#31291=DIRECTION('ref_axis',(0.353157342779898,0.,0.935563942892543));
#31292=DIRECTION('',(0.,1.,0.));
#31293=DIRECTION('center_axis',(-0.954992592290509,0.,0.296629649007399));
#31294=DIRECTION('ref_axis',(0.296629649007399,0.,0.954992592290509));
#31295=DIRECTION('',(0.,1.,0.));
#31296=DIRECTION('center_axis',(-0.971832145680527,0.,0.235674098326447));
#31297=DIRECTION('ref_axis',(0.235674098326447,0.,0.971832145680527));
#31298=DIRECTION('',(0.,1.,0.));
#31299=DIRECTION('center_axis',(-0.985571729311692,0.,0.169258283051554));
#31300=DIRECTION('ref_axis',(0.169258283051554,0.,0.985571729311692));
#31301=DIRECTION('',(0.,1.,0.));
#31302=DIRECTION('center_axis',(-0.995411093351309,0.,0.0956909360031101));
#31303=DIRECTION('ref_axis',(0.0956909360031101,0.,0.995411093351309));
#31304=DIRECTION('',(0.,1.,0.));
#31305=DIRECTION('center_axis',(-0.999929660354767,0.,0.0118606215182901));
#31306=DIRECTION('ref_axis',(0.0118606215182901,0.,0.999929660354767));
#31307=DIRECTION('',(0.,1.,0.));
#31308=DIRECTION('center_axis',(-0.996005310591038,0.,-0.0892940158938378));
#31309=DIRECTION('ref_axis',(-0.0892940158938378,0.,0.996005310591038));
#31310=DIRECTION('center_axis',(-0.454871137731935,0.,0.890557268264346));
#31311=DIRECTION('ref_axis',(0.890557268264346,0.,0.454871137731935));
#31312=DIRECTION('',(0.,1.,0.));
#31313=DIRECTION('center_axis',(-0.54380964897583,0.,0.839208594856359));
#31314=DIRECTION('ref_axis',(0.839208594856359,0.,0.54380964897583));
#31315=DIRECTION('',(0.,1.,0.));
#31316=DIRECTION('center_axis',(0.810177595661693,0.,0.586184496116912));
#31317=DIRECTION('ref_axis',(0.586184496116912,0.,-0.810177595661693));
#31318=DIRECTION('',(0.,1.,0.));
#31319=DIRECTION('center_axis',(0.69194085983215,0.,0.721954185869675));
#31320=DIRECTION('ref_axis',(0.721954185869675,0.,-0.69194085983215));
#31321=DIRECTION('center_axis',(0.414834765185043,0.,0.909896762052635));
#31322=DIRECTION('ref_axis',(0.909896762052635,0.,-0.414834765185043));
#31323=DIRECTION('',(0.,1.,0.));
#31324=DIRECTION('center_axis',(0.346203891732275,0.,0.938159296361459));
#31325=DIRECTION('ref_axis',(0.938159296361459,0.,-0.346203891732275));
#31326=DIRECTION('',(0.,1.,0.));
#31327=DIRECTION('center_axis',(0.281816316675565,0.,0.9594683755369));
#31328=DIRECTION('ref_axis',(0.9594683755369,0.,-0.281816316675565));
#31329=DIRECTION('',(0.,1.,0.));
#31330=DIRECTION('center_axis',(0.220607484589184,0.,0.975362669853236));
#31331=DIRECTION('ref_axis',(0.975362669853236,0.,-0.220607484589184));
#31332=DIRECTION('',(0.,1.,0.));
#31333=DIRECTION('center_axis',(0.161938741065868,0.,0.986800812799626));
#31334=DIRECTION('ref_axis',(0.986800812799626,0.,-0.161938741065868));
#31335=DIRECTION('',(0.,1.,0.));
#31336=DIRECTION('center_axis',(-0.691221298772308,0.,0.722643145766652));
#31337=DIRECTION('ref_axis',(0.722643145766652,0.,0.691221298772308));
#31338=DIRECTION('',(0.,1.,0.));
#31339=DIRECTION('center_axis',(-0.701850027448819,0.,0.712324742635051));
#31340=DIRECTION('ref_axis',(0.712324742635051,0.,0.701850027448819));
#31341=DIRECTION('',(0.,1.,0.));
#31342=DIRECTION('center_axis',(-0.712324742635055,0.,0.701850027448815));
#31343=DIRECTION('ref_axis',(0.701850027448815,0.,0.712324742635055));
#31344=DIRECTION('',(0.,1.,0.));
#31345=DIRECTION('center_axis',(-0.722643145766649,0.,0.691221298772312));
#31346=DIRECTION('ref_axis',(0.691221298772312,0.,0.722643145766649));
#31347=DIRECTION('',(0.,1.,0.));
#31348=DIRECTION('center_axis',(-0.986800812799626,0.,-0.161938741065865));
#31349=DIRECTION('ref_axis',(-0.161938741065865,0.,0.986800812799626));
#31350=DIRECTION('',(0.,1.,0.));
#31351=DIRECTION('center_axis',(-0.975362669853235,0.,-0.220607484589187));
#31352=DIRECTION('ref_axis',(-0.220607484589187,0.,0.975362669853235));
#31353=DIRECTION('',(0.,1.,0.));
#31354=DIRECTION('center_axis',(-0.9594683755369,0.,-0.281816316675565));
#31355=DIRECTION('ref_axis',(-0.281816316675565,0.,0.9594683755369));
#31356=DIRECTION('',(0.,1.,0.));
#31357=DIRECTION('center_axis',(-0.93815929636146,0.,-0.346203891732272));
#31358=DIRECTION('ref_axis',(-0.346203891732272,0.,0.93815929636146));
#31359=DIRECTION('',(0.,1.,0.));
#31360=DIRECTION('center_axis',(-0.909896762052633,0.,-0.414834765185049));
#31361=DIRECTION('ref_axis',(-0.414834765185049,0.,0.909896762052633));
#31362=DIRECTION('',(0.,1.,0.));
#31363=DIRECTION('center_axis',(-0.871894798623921,0.,-0.489693230637868));
#31364=DIRECTION('ref_axis',(-0.489693230637868,0.,0.871894798623921));
#31365=DIRECTION('',(0.,1.,0.));
#31366=DIRECTION('center_axis',(-0.817918893329128,0.,-0.575333541465517));
#31367=DIRECTION('ref_axis',(-0.575333541465517,0.,0.817918893329128));
#31368=DIRECTION('center_axis',(-0.839208594856358,0.,0.543809648975831));
#31369=DIRECTION('ref_axis',(0.543809648975831,0.,0.839208594856358));
#31370=DIRECTION('',(0.,1.,0.));
#31371=DIRECTION('center_axis',(-0.890557268264347,0.,0.454871137731934));
#31372=DIRECTION('ref_axis',(0.454871137731934,0.,0.890557268264347));
#31373=DIRECTION('',(0.,1.,0.));
#31374=DIRECTION('center_axis',(0.408542131361568,0.,0.912739462772673));
#31375=DIRECTION('ref_axis',(0.912739462772673,0.,-0.408542131361568));
#31376=DIRECTION('',(0.,1.,0.));
#31377=DIRECTION('center_axis',(0.238261269596254,0.,0.971201095247725));
#31378=DIRECTION('ref_axis',(0.971201095247725,0.,-0.238261269596254));
#31379=DIRECTION('center_axis',(-0.0956909360031137,0.,0.995411093351309));
#31380=DIRECTION('ref_axis',(0.995411093351309,0.,0.0956909360031137));
#31381=DIRECTION('',(0.,1.,0.));
#31382=DIRECTION('center_axis',(-0.169258283051549,0.,0.985571729311693));
#31383=DIRECTION('ref_axis',(0.985571729311693,0.,0.169258283051549));
#31384=DIRECTION('',(0.,1.,0.));
#31385=DIRECTION('center_axis',(-0.235674098326448,0.,0.971832145680526));
#31386=DIRECTION('ref_axis',(0.971832145680526,0.,0.235674098326448));
#31387=DIRECTION('',(0.,1.,0.));
#31388=DIRECTION('center_axis',(-0.296629649007392,0.,0.954992592290512));
#31389=DIRECTION('ref_axis',(0.954992592290512,0.,0.296629649007392));
#31390=DIRECTION('',(0.,1.,0.));
#31391=DIRECTION('center_axis',(-0.353157342779906,0.,0.93556394289254));
#31392=DIRECTION('ref_axis',(0.93556394289254,0.,0.353157342779906));
#31393=DIRECTION('',(0.,1.,0.));
#31394=DIRECTION('center_axis',(-0.95993677725702,0.,0.280216672718464));
#31395=DIRECTION('ref_axis',(0.280216672718464,0.,0.95993677725702));
#31396=DIRECTION('',(0.,1.,0.));
#31397=DIRECTION('center_axis',(-0.963982324735009,0.,0.265966309141754));
#31398=DIRECTION('ref_axis',(0.265966309141754,0.,0.963982324735009));
#31399=DIRECTION('',(0.,1.,0.));
#31400=DIRECTION('center_axis',(-0.967816336590576,0.,0.251657582099958));
#31401=DIRECTION('ref_axis',(0.251657582099958,0.,0.967816336590576));
#31402=DIRECTION('',(0.,1.,0.));
#31403=DIRECTION('center_axis',(-0.971437971490776,0.,0.237293631490368));
#31404=DIRECTION('ref_axis',(0.237293631490368,0.,0.971437971490776));
#31405=DIRECTION('',(0.,1.,0.));
#31406=DIRECTION('center_axis',(-0.773625201826675,0.,-0.633643470019724));
#31407=DIRECTION('ref_axis',(-0.633643470019724,0.,0.773625201826675));
#31408=DIRECTION('',(0.,1.,0.));
#31409=DIRECTION('center_axis',(-0.734385107701318,0.,-0.678733020845843));
#31410=DIRECTION('ref_axis',(-0.678733020845843,0.,0.734385107701318));
#31411=DIRECTION('',(0.,1.,0.));
#31412=DIRECTION('center_axis',(-0.690015829004965,0.,-0.723794277210445));
#31413=DIRECTION('ref_axis',(-0.723794277210445,0.,0.690015829004965));
#31414=DIRECTION('',(0.,1.,0.));
#31415=DIRECTION('center_axis',(-0.639367837579419,0.,-0.768901013309918));
#31416=DIRECTION('ref_axis',(-0.768901013309918,0.,0.639367837579419));
#31417=DIRECTION('',(0.,1.,0.));
#31418=DIRECTION('center_axis',(-0.580576328166263,0.,-0.814205826049519));
#31419=DIRECTION('ref_axis',(-0.814205826049519,0.,0.580576328166263));
#31420=DIRECTION('',(0.,1.,0.));
#31421=DIRECTION('center_axis',(-0.510236429716893,0.,-0.86003417710563));
#31422=DIRECTION('ref_axis',(-0.86003417710563,0.,0.510236429716893));
#31423=DIRECTION('',(0.,1.,0.));
#31424=DIRECTION('center_axis',(-0.420671769125522,0.,-0.907212909222969));
#31425=DIRECTION('ref_axis',(-0.907212909222969,0.,0.420671769125522));
#31426=DIRECTION('center_axis',(-0.998680786707765,0.,0.0513486734079878));
#31427=DIRECTION('ref_axis',(0.0513486734079878,0.,0.998680786707765));
#31428=DIRECTION('',(0.,1.,0.));
#31429=DIRECTION('center_axis',(-0.998680786707765,0.,-0.0513486734079878));
#31430=DIRECTION('ref_axis',(-0.0513486734079878,0.,0.998680786707765));
#31431=DIRECTION('',(0.,1.,0.));
#31432=DIRECTION('center_axis',(-0.102561867110979,0.,0.99472662747848));
#31433=DIRECTION('ref_axis',(0.99472662747848,0.,0.102561867110979));
#31434=DIRECTION('',(0.,1.,0.));
#31435=DIRECTION('center_axis',(-0.279260235415588,0.,0.960215455465923));
#31436=DIRECTION('ref_axis',(0.960215455465923,0.,0.279260235415588));
#31437=DIRECTION('center_axis',(-0.580576328166259,0.,0.814205826049522));
#31438=DIRECTION('ref_axis',(0.814205826049522,0.,0.580576328166259));
#31439=DIRECTION('',(0.,1.,0.));
#31440=DIRECTION('center_axis',(-0.639367837579427,0.,0.768901013309911));
#31441=DIRECTION('ref_axis',(0.768901013309911,0.,0.639367837579427));
#31442=DIRECTION('',(0.,1.,0.));
#31443=DIRECTION('center_axis',(-0.690015829004956,0.,0.723794277210454));
#31444=DIRECTION('ref_axis',(0.723794277210454,0.,0.690015829004956));
#31445=DIRECTION('',(0.,1.,0.));
#31446=DIRECTION('center_axis',(-0.734385107701322,0.,0.678733020845838));
#31447=DIRECTION('ref_axis',(0.678733020845838,0.,0.734385107701322));
#31448=DIRECTION('',(0.,1.,0.));
#31449=DIRECTION('center_axis',(-0.773625201826678,0.,0.63364347001972));
#31450=DIRECTION('ref_axis',(0.63364347001972,0.,0.773625201826678));
#31451=DIRECTION('',(0.,1.,0.));
#31452=DIRECTION('center_axis',(-0.971437971490779,0.,-0.237293631490357));
#31453=DIRECTION('ref_axis',(-0.237293631490357,0.,0.971437971490779));
#31454=DIRECTION('',(0.,1.,0.));
#31455=DIRECTION('center_axis',(-0.967816336590576,0.,-0.251657582099958));
#31456=DIRECTION('ref_axis',(-0.251657582099958,0.,0.967816336590576));
#31457=DIRECTION('',(0.,1.,0.));
#31458=DIRECTION('center_axis',(-0.963982324735009,0.,-0.265966309141754));
#31459=DIRECTION('ref_axis',(-0.265966309141754,0.,0.963982324735009));
#31460=DIRECTION('',(0.,1.,0.));
#31461=DIRECTION('center_axis',(-0.959936777257016,0.,-0.280216672718478));
#31462=DIRECTION('ref_axis',(-0.280216672718478,0.,0.959936777257016));
#31463=DIRECTION('',(0.,1.,0.));
#31464=DIRECTION('center_axis',(-0.3531573427799,0.,-0.935563942892542));
#31465=DIRECTION('ref_axis',(-0.935563942892542,0.,0.3531573427799));
#31466=DIRECTION('',(0.,1.,0.));
#31467=DIRECTION('center_axis',(-0.296629649007398,0.,-0.95499259229051));
#31468=DIRECTION('ref_axis',(-0.95499259229051,0.,0.296629649007398));
#31469=DIRECTION('',(0.,1.,0.));
#31470=DIRECTION('center_axis',(-0.235674098326456,0.,-0.971832145680524));
#31471=DIRECTION('ref_axis',(-0.971832145680524,0.,0.235674098326456));
#31472=DIRECTION('',(0.,1.,0.));
#31473=DIRECTION('center_axis',(-0.169258283051542,0.,-0.985571729311695));
#31474=DIRECTION('ref_axis',(-0.985571729311695,0.,0.169258283051542));
#31475=DIRECTION('',(0.,1.,0.));
#31476=DIRECTION('center_axis',(-0.0956909360031057,0.,-0.99541109335131));
#31477=DIRECTION('ref_axis',(-0.99541109335131,0.,0.0956909360031057));
#31478=DIRECTION('',(0.,1.,0.));
#31479=DIRECTION('center_axis',(-0.011860621518292,0.,-0.999929660354767));
#31480=DIRECTION('ref_axis',(-0.999929660354767,0.,0.011860621518292));
#31481=DIRECTION('',(0.,1.,0.));
#31482=DIRECTION('center_axis',(0.0892940158938382,0.,-0.996005310591038));
#31483=DIRECTION('ref_axis',(-0.996005310591038,0.,-0.0892940158938382));
#31484=DIRECTION('center_axis',(-0.890557268264347,0.,-0.454871137731934));
#31485=DIRECTION('ref_axis',(-0.454871137731934,0.,0.890557268264347));
#31486=DIRECTION('',(0.,1.,0.));
#31487=DIRECTION('center_axis',(-0.839208594856358,0.,-0.543809648975832));
#31488=DIRECTION('ref_axis',(-0.543809648975832,0.,0.839208594856358));
#31489=DIRECTION('',(0.,1.,0.));
#31490=DIRECTION('center_axis',(-0.586184496116913,0.,0.810177595661692));
#31491=DIRECTION('ref_axis',(0.810177595661692,0.,0.586184496116913));
#31492=DIRECTION('',(0.,1.,0.));
#31493=DIRECTION('center_axis',(-0.72195418586968,0.,0.691940859832145));
#31494=DIRECTION('ref_axis',(0.691940859832145,0.,0.72195418586968));
#31495=DIRECTION('center_axis',(-0.909896762052634,0.,0.414834765185046));
#31496=DIRECTION('ref_axis',(0.414834765185046,0.,0.909896762052634));
#31497=DIRECTION('',(0.,1.,0.));
#31498=DIRECTION('center_axis',(-0.938159296361461,0.,0.346203891732269));
#31499=DIRECTION('ref_axis',(0.346203891732269,0.,0.938159296361461));
#31500=DIRECTION('',(0.,1.,0.));
#31501=DIRECTION('center_axis',(-0.9594683755369,0.,0.281816316675564));
#31502=DIRECTION('ref_axis',(0.281816316675564,0.,0.9594683755369));
#31503=DIRECTION('',(0.,1.,0.));
#31504=DIRECTION('center_axis',(-0.975362669853235,0.,0.22060748458919));
#31505=DIRECTION('ref_axis',(0.22060748458919,0.,0.975362669853235));
#31506=DIRECTION('',(0.,1.,0.));
#31507=DIRECTION('center_axis',(-0.986800812799626,0.,0.161938741065865));
#31508=DIRECTION('ref_axis',(0.161938741065865,0.,0.986800812799626));
#31509=DIRECTION('',(0.,1.,0.));
#31510=DIRECTION('center_axis',(-0.722643145766667,0.,-0.691221298772293));
#31511=DIRECTION('ref_axis',(-0.691221298772293,0.,0.722643145766667));
#31512=DIRECTION('',(0.,1.,0.));
#31513=DIRECTION('center_axis',(-0.712324742635048,0.,-0.701850027448823));
#31514=DIRECTION('ref_axis',(-0.701850027448823,0.,0.712324742635048));
#31515=DIRECTION('',(0.,1.,0.));
#31516=DIRECTION('center_axis',(-0.701850027448831,0.,-0.71232474263504));
#31517=DIRECTION('ref_axis',(-0.71232474263504,0.,0.701850027448831));
#31518=DIRECTION('',(0.,1.,0.));
#31519=DIRECTION('center_axis',(-0.691221298772292,0.,-0.722643145766668));
#31520=DIRECTION('ref_axis',(-0.722643145766668,0.,0.691221298772292));
#31521=DIRECTION('',(0.,1.,0.));
#31522=DIRECTION('center_axis',(0.161938741065863,0.,-0.986800812799627));
#31523=DIRECTION('ref_axis',(-0.986800812799626,0.,-0.161938741065863));
#31524=DIRECTION('',(0.,1.,0.));
#31525=DIRECTION('center_axis',(0.2206074845892,0.,-0.975362669853233));
#31526=DIRECTION('ref_axis',(-0.975362669853233,0.,-0.2206074845892));
#31527=DIRECTION('',(0.,1.,0.));
#31528=DIRECTION('center_axis',(0.281816316675571,0.,-0.959468375536898));
#31529=DIRECTION('ref_axis',(-0.959468375536898,0.,-0.281816316675571));
#31530=DIRECTION('',(0.,1.,0.));
#31531=DIRECTION('center_axis',(0.346203891732263,0.,-0.938159296361463));
#31532=DIRECTION('ref_axis',(-0.938159296361463,0.,-0.346203891732263));
#31533=DIRECTION('',(0.,1.,0.));
#31534=DIRECTION('center_axis',(0.414834765185061,0.,-0.909896762052627));
#31535=DIRECTION('ref_axis',(-0.909896762052627,0.,-0.414834765185061));
#31536=DIRECTION('',(0.,1.,0.));
#31537=DIRECTION('center_axis',(0.48969323063784,0.,-0.871894798623937));
#31538=DIRECTION('ref_axis',(-0.871894798623937,0.,-0.48969323063784));
#31539=DIRECTION('',(0.,1.,0.));
#31540=DIRECTION('center_axis',(0.575333541465521,0.,-0.817918893329125));
#31541=DIRECTION('ref_axis',(-0.817918893329125,0.,-0.575333541465521));
#31542=DIRECTION('center_axis',(-0.543809648975832,0.,-0.839208594856358));
#31543=DIRECTION('ref_axis',(-0.839208594856358,0.,0.543809648975832));
#31544=DIRECTION('',(0.,1.,0.));
#31545=DIRECTION('center_axis',(-0.454871137731935,0.,-0.890557268264346));
#31546=DIRECTION('ref_axis',(-0.890557268264346,0.,0.454871137731935));
#31547=DIRECTION('',(0.,1.,0.));
#31548=DIRECTION('center_axis',(-0.912739462772673,0.,0.408542131361568));
#31549=DIRECTION('ref_axis',(0.408542131361568,0.,0.912739462772673));
#31550=DIRECTION('',(0.,1.,0.));
#31551=DIRECTION('center_axis',(-0.971201095247723,0.,0.238261269596262));
#31552=DIRECTION('ref_axis',(0.238261269596262,0.,0.971201095247723));
#31553=DIRECTION('center_axis',(-0.99541109335131,0.,-0.0956909360031021));
#31554=DIRECTION('ref_axis',(-0.0956909360031021,0.,0.99541109335131));
#31555=DIRECTION('',(0.,1.,0.));
#31556=DIRECTION('center_axis',(-0.985571729311692,0.,-0.169258283051555));
#31557=DIRECTION('ref_axis',(-0.169258283051555,0.,0.985571729311692));
#31558=DIRECTION('',(0.,1.,0.));
#31559=DIRECTION('center_axis',(-0.97183214568053,0.,-0.235674098326432));
#31560=DIRECTION('ref_axis',(-0.235674098326432,0.,0.97183214568053));
#31561=DIRECTION('',(0.,1.,0.));
#31562=DIRECTION('center_axis',(-0.954992592290506,0.,-0.296629649007409));
#31563=DIRECTION('ref_axis',(-0.296629649007409,0.,0.954992592290506));
#31564=DIRECTION('',(0.,1.,0.));
#31565=DIRECTION('center_axis',(-0.935563942892542,0.,-0.3531573427799));
#31566=DIRECTION('ref_axis',(-0.3531573427799,0.,0.935563942892542));
#31567=DIRECTION('',(0.,1.,0.));
#31568=DIRECTION('center_axis',(-0.280216672718486,0.,-0.959936777257014));
#31569=DIRECTION('ref_axis',(-0.959936777257014,0.,0.280216672718486));
#31570=DIRECTION('',(0.,1.,0.));
#31571=DIRECTION('center_axis',(-0.265966309141761,0.,-0.963982324735007));
#31572=DIRECTION('ref_axis',(-0.963982324735007,0.,0.265966309141761));
#31573=DIRECTION('',(0.,1.,0.));
#31574=DIRECTION('center_axis',(-0.251657582099936,0.,-0.967816336590582));
#31575=DIRECTION('ref_axis',(-0.967816336590582,0.,0.251657582099936));
#31576=DIRECTION('',(0.,1.,0.));
#31577=DIRECTION('center_axis',(-0.237293631490379,0.,-0.971437971490773));
#31578=DIRECTION('ref_axis',(-0.971437971490773,0.,0.237293631490379));
#31579=DIRECTION('',(0.,1.,0.));
#31580=DIRECTION('center_axis',(0.633643470019722,0.,-0.773625201826676));
#31581=DIRECTION('ref_axis',(-0.773625201826676,0.,-0.633643470019722));
#31582=DIRECTION('',(0.,1.,0.));
#31583=DIRECTION('center_axis',(0.678733020845836,0.,-0.734385107701325));
#31584=DIRECTION('ref_axis',(-0.734385107701325,0.,-0.678733020845836));
#31585=DIRECTION('',(0.,1.,0.));
#31586=DIRECTION('center_axis',(0.723794277210459,0.,-0.69001582900495));
#31587=DIRECTION('ref_axis',(-0.69001582900495,0.,-0.723794277210459));
#31588=DIRECTION('',(0.,1.,0.));
#31589=DIRECTION('center_axis',(0.768901013309907,0.,-0.639367837579431));
#31590=DIRECTION('ref_axis',(-0.639367837579431,0.,-0.768901013309907));
#31591=DIRECTION('',(0.,1.,0.));
#31592=DIRECTION('center_axis',(0.814205826049531,0.,-0.580576328166246));
#31593=DIRECTION('ref_axis',(-0.580576328166246,0.,-0.814205826049531));
#31594=DIRECTION('',(0.,1.,0.));
#31595=DIRECTION('center_axis',(0.860034177105626,0.,-0.510236429716899));
#31596=DIRECTION('ref_axis',(-0.510236429716899,0.,-0.860034177105626));
#31597=DIRECTION('',(0.,1.,0.));
#31598=DIRECTION('center_axis',(0.907212909222961,0.,-0.42067176912554));
#31599=DIRECTION('ref_axis',(-0.42067176912554,0.,-0.907212909222961));
#31600=DIRECTION('center_axis',(-0.0513486734079864,0.,-0.998680786707765));
#31601=DIRECTION('ref_axis',(-0.998680786707765,0.,0.0513486734079864));
#31602=DIRECTION('',(0.,1.,0.));
#31603=DIRECTION('center_axis',(0.0513486734079863,0.,-0.998680786707765));
#31604=DIRECTION('ref_axis',(-0.998680786707765,0.,-0.0513486734079863));
#31605=DIRECTION('',(0.,1.,0.));
#31606=DIRECTION('center_axis',(-0.99472662747848,0.,-0.102561867110979));
#31607=DIRECTION('ref_axis',(-0.102561867110979,0.,0.99472662747848));
#31608=DIRECTION('',(0.,1.,0.));
#31609=DIRECTION('center_axis',(-0.960215455465929,0.,-0.279260235415567));
#31610=DIRECTION('ref_axis',(-0.279260235415567,0.,0.960215455465929));
#31611=DIRECTION('center_axis',(-0.814205826049532,0.,-0.580576328166246));
#31612=DIRECTION('ref_axis',(-0.580576328166246,0.,0.814205826049532));
#31613=DIRECTION('',(0.,1.,0.));
#31614=DIRECTION('center_axis',(-0.768901013309908,0.,-0.639367837579431));
#31615=DIRECTION('ref_axis',(-0.639367837579431,0.,0.768901013309908));
#31616=DIRECTION('',(0.,1.,0.));
#31617=DIRECTION('center_axis',(-0.723794277210459,0.,-0.69001582900495));
#31618=DIRECTION('ref_axis',(-0.69001582900495,0.,0.723794277210459));
#31619=DIRECTION('',(0.,1.,0.));
#31620=DIRECTION('center_axis',(-0.678733020845836,0.,-0.734385107701325));
#31621=DIRECTION('ref_axis',(-0.734385107701325,0.,0.678733020845836));
#31622=DIRECTION('',(0.,1.,0.));
#31623=DIRECTION('center_axis',(-0.63364347001973,0.,-0.77362520182667));
#31624=DIRECTION('ref_axis',(-0.77362520182667,0.,0.63364347001973));
#31625=DIRECTION('',(0.,1.,0.));
#31626=DIRECTION('center_axis',(0.237293631490407,0.,-0.971437971490766));
#31627=DIRECTION('ref_axis',(-0.971437971490766,0.,-0.237293631490407));
#31628=DIRECTION('',(0.,1.,0.));
#31629=DIRECTION('center_axis',(0.251657582099936,0.,-0.967816336590582));
#31630=DIRECTION('ref_axis',(-0.967816336590582,0.,-0.251657582099936));
#31631=DIRECTION('',(0.,1.,0.));
#31632=DIRECTION('center_axis',(0.265966309141763,0.,-0.963982324735007));
#31633=DIRECTION('ref_axis',(-0.963982324735007,0.,-0.265966309141763));
#31634=DIRECTION('',(0.,1.,0.));
#31635=DIRECTION('center_axis',(0.280216672718455,0.,-0.959936777257023));
#31636=DIRECTION('ref_axis',(-0.959936777257023,0.,-0.280216672718455));
#31637=DIRECTION('',(0.,1.,0.));
#31638=DIRECTION('center_axis',(0.935563942892543,0.,-0.353157342779899));
#31639=DIRECTION('ref_axis',(-0.353157342779899,0.,-0.935563942892543));
#31640=DIRECTION('',(0.,1.,0.));
#31641=DIRECTION('center_axis',(0.954992592290507,0.,-0.296629649007407));
#31642=DIRECTION('ref_axis',(-0.296629649007407,0.,-0.954992592290507));
#31643=DIRECTION('',(0.,1.,0.));
#31644=DIRECTION('center_axis',(0.97183214568053,0.,-0.235674098326432));
#31645=DIRECTION('ref_axis',(-0.235674098326432,0.,-0.97183214568053));
#31646=DIRECTION('',(0.,1.,0.));
#31647=DIRECTION('center_axis',(0.985571729311692,0.,-0.169258283051555));
#31648=DIRECTION('ref_axis',(-0.169258283051555,0.,-0.985571729311692));
#31649=DIRECTION('',(0.,1.,0.));
#31650=DIRECTION('center_axis',(0.99541109335131,0.,-0.0956909360031021));
#31651=DIRECTION('ref_axis',(-0.0956909360031021,0.,-0.99541109335131));
#31652=DIRECTION('',(0.,1.,0.));
#31653=DIRECTION('center_axis',(0.999929660354767,0.,-0.0118606215182939));
#31654=DIRECTION('ref_axis',(-0.0118606215182939,0.,-0.999929660354767));
#31655=DIRECTION('',(0.,1.,0.));
#31656=DIRECTION('center_axis',(0.99600531059104,0.,0.0892940158938226));
#31657=DIRECTION('ref_axis',(0.0892940158938226,0.,-0.99600531059104));
#31658=DIRECTION('center_axis',(0.45487113773193,0.,-0.890557268264349));
#31659=DIRECTION('ref_axis',(-0.890557268264349,0.,-0.45487113773193));
#31660=DIRECTION('',(0.,1.,0.));
#31661=DIRECTION('center_axis',(0.543809648975832,0.,-0.839208594856358));
#31662=DIRECTION('ref_axis',(-0.839208594856358,0.,-0.543809648975832));
#31663=DIRECTION('',(0.,1.,0.));
#31664=DIRECTION('center_axis',(-0.810177595661693,0.,-0.586184496116913));
#31665=DIRECTION('ref_axis',(-0.586184496116913,0.,0.810177595661693));
#31666=DIRECTION('',(0.,1.,0.));
#31667=DIRECTION('center_axis',(-0.691940859832157,0.,-0.721954185869668));
#31668=DIRECTION('ref_axis',(-0.721954185869668,0.,0.691940859832157));
#31669=DIRECTION('center_axis',(-0.41483476518505,0.,-0.909896762052632));
#31670=DIRECTION('ref_axis',(-0.909896762052632,0.,0.41483476518505));
#31671=DIRECTION('',(0.,1.,0.));
#31672=DIRECTION('center_axis',(-0.346203891732262,0.,-0.938159296361464));
#31673=DIRECTION('ref_axis',(-0.938159296361463,0.,0.346203891732262));
#31674=DIRECTION('',(0.,1.,0.));
#31675=DIRECTION('center_axis',(-0.2818163166756,0.,-0.95946837553689));
#31676=DIRECTION('ref_axis',(-0.95946837553689,0.,0.2818163166756));
#31677=DIRECTION('',(0.,1.,0.));
#31678=DIRECTION('center_axis',(-0.220607484589173,0.,-0.975362669853239));
#31679=DIRECTION('ref_axis',(-0.975362669853239,0.,0.220607484589173));
#31680=DIRECTION('',(0.,1.,0.));
#31681=DIRECTION('center_axis',(-0.161938741065875,0.,-0.986800812799625));
#31682=DIRECTION('ref_axis',(-0.986800812799624,0.,0.161938741065875));
#31683=DIRECTION('',(0.,1.,0.));
#31684=DIRECTION('center_axis',(0.691221298772324,0.,-0.722643145766637));
#31685=DIRECTION('ref_axis',(-0.722643145766637,0.,-0.691221298772324));
#31686=DIRECTION('',(0.,1.,0.));
#31687=DIRECTION('center_axis',(0.701850027448807,0.,-0.712324742635063));
#31688=DIRECTION('ref_axis',(-0.712324742635063,0.,-0.701850027448807));
#31689=DIRECTION('',(0.,1.,0.));
#31690=DIRECTION('center_axis',(0.712324742635063,0.,-0.701850027448807));
#31691=DIRECTION('ref_axis',(-0.701850027448807,0.,-0.712324742635063));
#31692=DIRECTION('',(0.,1.,0.));
#31693=DIRECTION('center_axis',(0.722643145766645,0.,-0.691221298772316));
#31694=DIRECTION('ref_axis',(-0.691221298772316,0.,-0.722643145766645));
#31695=DIRECTION('',(0.,1.,0.));
#31696=DIRECTION('center_axis',(0.986800812799627,0.,0.161938741065862));
#31697=DIRECTION('ref_axis',(0.161938741065862,0.,-0.986800812799627));
#31698=DIRECTION('',(0.,1.,0.));
#31699=DIRECTION('center_axis',(0.975362669853236,0.,0.220607484589184));
#31700=DIRECTION('ref_axis',(0.220607484589184,0.,-0.975362669853236));
#31701=DIRECTION('',(0.,1.,0.));
#31702=DIRECTION('center_axis',(0.959468375536897,0.,0.281816316675577));
#31703=DIRECTION('ref_axis',(0.281816316675577,0.,-0.959468375536896));
#31704=DIRECTION('',(0.,1.,0.));
#31705=DIRECTION('center_axis',(0.938159296361463,0.,0.346203891732263));
#31706=DIRECTION('ref_axis',(0.346203891732263,0.,-0.938159296361463));
#31707=DIRECTION('',(0.,1.,0.));
#31708=DIRECTION('center_axis',(0.909896762052627,0.,0.414834765185061));
#31709=DIRECTION('ref_axis',(0.414834765185061,0.,-0.909896762052627));
#31710=DIRECTION('',(0.,1.,0.));
#31711=DIRECTION('center_axis',(0.871894798623931,0.,0.48969323063785));
#31712=DIRECTION('ref_axis',(0.48969323063785,0.,-0.871894798623931));
#31713=DIRECTION('',(0.,1.,0.));
#31714=DIRECTION('center_axis',(0.817918893329121,0.,0.575333541465527));
#31715=DIRECTION('ref_axis',(0.575333541465527,0.,-0.817918893329121));
#31716=DIRECTION('center_axis',(0.839208594856359,0.,-0.543809648975831));
#31717=DIRECTION('ref_axis',(-0.543809648975831,0.,-0.839208594856359));
#31718=DIRECTION('',(0.,1.,0.));
#31719=DIRECTION('center_axis',(0.890557268264347,0.,-0.454871137731933));
#31720=DIRECTION('ref_axis',(-0.454871137731933,0.,-0.890557268264347));
#31721=DIRECTION('',(0.,1.,0.));
#31722=DIRECTION('center_axis',(-0.408542131361568,0.,-0.912739462772673));
#31723=DIRECTION('ref_axis',(-0.912739462772673,0.,0.408542131361568));
#31724=DIRECTION('',(0.,1.,0.));
#31725=DIRECTION('center_axis',(-0.238261269596263,0.,-0.971201095247723));
#31726=DIRECTION('ref_axis',(-0.971201095247723,0.,0.238261269596263));
#31727=DIRECTION('center_axis',(0.0956909360030992,0.,-0.99541109335131));
#31728=DIRECTION('ref_axis',(-0.99541109335131,0.,-0.0956909360030991));
#31729=DIRECTION('',(0.,1.,0.));
#31730=DIRECTION('center_axis',(0.169258283051569,0.,-0.98557172931169));
#31731=DIRECTION('ref_axis',(-0.98557172931169,0.,-0.169258283051569));
#31732=DIRECTION('',(0.,1.,0.));
#31733=DIRECTION('center_axis',(0.235674098326418,0.,-0.971832145680534));
#31734=DIRECTION('ref_axis',(-0.971832145680534,0.,-0.235674098326418));
#31735=DIRECTION('',(0.,1.,0.));
#31736=DIRECTION('center_axis',(0.29662964900741,0.,-0.954992592290506));
#31737=DIRECTION('ref_axis',(-0.954992592290506,0.,-0.29662964900741));
#31738=DIRECTION('',(0.,1.,0.));
#31739=DIRECTION('center_axis',(0.3531573427799,0.,-0.935563942892542));
#31740=DIRECTION('ref_axis',(-0.935563942892542,0.,-0.3531573427799));
#31741=DIRECTION('',(0.,1.,0.));
#31742=DIRECTION('center_axis',(0.959936777257017,0.,-0.280216672718472));
#31743=DIRECTION('ref_axis',(-0.280216672718472,0.,-0.959936777257017));
#31744=DIRECTION('',(0.,1.,0.));
#31745=DIRECTION('center_axis',(0.963982324735009,0.,-0.265966309141757));
#31746=DIRECTION('ref_axis',(-0.265966309141757,0.,-0.963982324735009));
#31747=DIRECTION('',(0.,1.,0.));
#31748=DIRECTION('center_axis',(0.967816336590577,0.,-0.251657582099955));
#31749=DIRECTION('ref_axis',(-0.251657582099955,0.,-0.967816336590577));
#31750=DIRECTION('',(0.,1.,0.));
#31751=DIRECTION('center_axis',(0.971437971490778,0.,-0.237293631490361));
#31752=DIRECTION('ref_axis',(-0.237293631490361,0.,-0.971437971490778));
#31753=DIRECTION('',(0.,1.,0.));
#31754=DIRECTION('center_axis',(0.773625201826675,0.,0.633643470019724));
#31755=DIRECTION('ref_axis',(0.633643470019724,0.,-0.773625201826675));
#31756=DIRECTION('',(0.,1.,0.));
#31757=DIRECTION('center_axis',(0.734385107701329,0.,0.678733020845831));
#31758=DIRECTION('ref_axis',(0.678733020845831,0.,-0.734385107701329));
#31759=DIRECTION('',(0.,1.,0.));
#31760=DIRECTION('center_axis',(0.690015829004945,0.,0.723794277210464));
#31761=DIRECTION('ref_axis',(0.723794277210464,0.,-0.690015829004945));
#31762=DIRECTION('',(0.,1.,0.));
#31763=DIRECTION('center_axis',(0.639367837579431,0.,0.768901013309907));
#31764=DIRECTION('ref_axis',(0.768901013309907,0.,-0.639367837579431));
#31765=DIRECTION('',(0.,1.,0.));
#31766=DIRECTION('center_axis',(0.580576328166249,0.,0.814205826049529));
#31767=DIRECTION('ref_axis',(0.814205826049529,0.,-0.580576328166249));
#31768=DIRECTION('',(0.,1.,0.));
#31769=DIRECTION('center_axis',(0.510236429716898,0.,0.860034177105627));
#31770=DIRECTION('ref_axis',(0.860034177105627,0.,-0.510236429716898));
#31771=DIRECTION('',(0.,1.,0.));
#31772=DIRECTION('center_axis',(0.420671769125548,0.,0.907212909222957));
#31773=DIRECTION('ref_axis',(0.907212909222957,0.,-0.420671769125548));
#31774=DIRECTION('center_axis',(0.998680786707765,0.,-0.0513486734079878));
#31775=DIRECTION('ref_axis',(-0.0513486734079878,0.,-0.998680786707765));
#31776=DIRECTION('',(0.,1.,0.));
#31777=DIRECTION('center_axis',(0.998680786707765,0.,0.0513486734079865));
#31778=DIRECTION('ref_axis',(0.0513486734079865,0.,-0.998680786707765));
#31779=DIRECTION('',(0.,1.,0.));
#31780=DIRECTION('center_axis',(0.102561867110979,0.,-0.99472662747848));
#31781=DIRECTION('ref_axis',(-0.99472662747848,0.,-0.102561867110979));
#31782=DIRECTION('',(0.,1.,0.));
#31783=DIRECTION('center_axis',(0.279260235415567,0.,-0.960215455465929));
#31784=DIRECTION('ref_axis',(-0.960215455465929,0.,-0.279260235415567));
#31785=DIRECTION('center_axis',(0.580576328166254,0.,-0.814205826049526));
#31786=DIRECTION('ref_axis',(-0.814205826049526,0.,-0.580576328166254));
#31787=DIRECTION('',(0.,1.,0.));
#31788=DIRECTION('center_axis',(0.639367837579427,0.,-0.768901013309911));
#31789=DIRECTION('ref_axis',(-0.768901013309911,0.,-0.639367837579427));
#31790=DIRECTION('',(0.,1.,0.));
#31791=DIRECTION('center_axis',(0.690015829004942,0.,-0.723794277210468));
#31792=DIRECTION('ref_axis',(-0.723794277210468,0.,-0.690015829004942));
#31793=DIRECTION('',(0.,1.,0.));
#31794=DIRECTION('center_axis',(0.734385107701332,0.,-0.678733020845828));
#31795=DIRECTION('ref_axis',(-0.678733020845828,0.,-0.734385107701332));
#31796=DIRECTION('',(0.,1.,0.));
#31797=DIRECTION('center_axis',(0.773625201826672,0.,-0.633643470019728));
#31798=DIRECTION('ref_axis',(-0.633643470019728,0.,-0.773625201826672));
#31799=DIRECTION('',(0.,1.,0.));
#31800=DIRECTION('center_axis',(0.971437971490777,0.,0.237293631490364));
#31801=DIRECTION('ref_axis',(0.237293631490364,0.,-0.971437971490777));
#31802=DIRECTION('',(0.,1.,0.));
#31803=DIRECTION('center_axis',(0.967816336590574,0.,0.251657582099965));
#31804=DIRECTION('ref_axis',(0.251657582099965,0.,-0.967816336590574));
#31805=DIRECTION('',(0.,1.,0.));
#31806=DIRECTION('center_axis',(0.963982324735012,0.,0.265966309141746));
#31807=DIRECTION('ref_axis',(0.265966309141746,0.,-0.963982324735012));
#31808=DIRECTION('',(0.,1.,0.));
#31809=DIRECTION('center_axis',(0.959936777257017,0.,0.280216672718472));
#31810=DIRECTION('ref_axis',(0.280216672718472,0.,-0.959936777257017));
#31811=DIRECTION('',(0.,1.,0.));
#31812=DIRECTION('center_axis',(0.353157342779907,0.,0.93556394289254));
#31813=DIRECTION('ref_axis',(0.93556394289254,0.,-0.353157342779907));
#31814=DIRECTION('',(0.,1.,0.));
#31815=DIRECTION('center_axis',(0.29662964900741,0.,0.954992592290506));
#31816=DIRECTION('ref_axis',(0.954992592290506,0.,-0.29662964900741));
#31817=DIRECTION('',(0.,1.,0.));
#31818=DIRECTION('center_axis',(0.235674098326429,0.,0.971832145680531));
#31819=DIRECTION('ref_axis',(0.971832145680531,0.,-0.235674098326429));
#31820=DIRECTION('',(0.,1.,0.));
#31821=DIRECTION('center_axis',(0.169258283051549,0.,0.985571729311693));
#31822=DIRECTION('ref_axis',(0.985571729311693,0.,-0.169258283051549));
#31823=DIRECTION('',(0.,1.,0.));
#31824=DIRECTION('center_axis',(0.0956909360031064,0.,0.99541109335131));
#31825=DIRECTION('ref_axis',(0.995411093351309,0.,-0.0956909360031064));
#31826=DIRECTION('',(0.,1.,0.));
#31827=DIRECTION('center_axis',(0.0118606215182996,0.,0.999929660354767));
#31828=DIRECTION('ref_axis',(0.999929660354767,0.,-0.0118606215182996));
#31829=DIRECTION('',(0.,1.,0.));
#31830=DIRECTION('center_axis',(-0.0892940158938297,0.,0.996005310591039));
#31831=DIRECTION('ref_axis',(0.996005310591039,0.,0.0892940158938297));
#31832=DIRECTION('center_axis',(0.890557268264347,0.,0.454871137731933));
#31833=DIRECTION('ref_axis',(0.454871137731933,0.,-0.890557268264347));
#31834=DIRECTION('',(0.,1.,0.));
#31835=DIRECTION('center_axis',(0.839208594856359,0.,0.54380964897583));
#31836=DIRECTION('ref_axis',(0.54380964897583,0.,-0.839208594856359));
#31837=DIRECTION('',(0.,1.,0.));
#31838=DIRECTION('center_axis',(0.586184496116911,0.,-0.810177595661694));
#31839=DIRECTION('ref_axis',(-0.810177595661694,0.,-0.586184496116911));
#31840=DIRECTION('',(0.,1.,0.));
#31841=DIRECTION('center_axis',(0.721954185869668,0.,-0.691940859832157));
#31842=DIRECTION('ref_axis',(-0.691940859832157,0.,-0.721954185869668));
#31843=DIRECTION('center_axis',(0.909896762052629,0.,-0.414834765185058));
#31844=DIRECTION('ref_axis',(-0.414834765185058,0.,-0.909896762052629));
#31845=DIRECTION('',(0.,1.,0.));
#31846=DIRECTION('center_axis',(0.938159296361463,0.,-0.346203891732264));
#31847=DIRECTION('ref_axis',(-0.346203891732264,0.,-0.938159296361463));
#31848=DIRECTION('',(0.,1.,0.));
#31849=DIRECTION('center_axis',(0.959468375536894,0.,-0.281816316675586));
#31850=DIRECTION('ref_axis',(-0.281816316675586,0.,-0.959468375536894));
#31851=DIRECTION('',(0.,1.,0.));
#31852=DIRECTION('center_axis',(0.975362669853238,0.,-0.220607484589178));
#31853=DIRECTION('ref_axis',(-0.220607484589178,0.,-0.975362669853237));
#31854=DIRECTION('',(0.,1.,0.));
#31855=DIRECTION('center_axis',(0.986800812799626,0.,-0.161938741065869));
#31856=DIRECTION('ref_axis',(-0.161938741065869,0.,-0.986800812799626));
#31857=DIRECTION('',(0.,1.,0.));
#31858=DIRECTION('center_axis',(0.722643145766656,0.,0.691221298772304));
#31859=DIRECTION('ref_axis',(0.691221298772304,0.,-0.722643145766656));
#31860=DIRECTION('',(0.,1.,0.));
#31861=DIRECTION('center_axis',(0.712324742635051,0.,0.701850027448819));
#31862=DIRECTION('ref_axis',(0.701850027448819,0.,-0.712324742635051));
#31863=DIRECTION('',(0.,1.,0.));
#31864=DIRECTION('center_axis',(0.701850027448819,0.,0.712324742635051));
#31865=DIRECTION('ref_axis',(0.712324742635051,0.,-0.701850027448819));
#31866=DIRECTION('',(0.,1.,0.));
#31867=DIRECTION('center_axis',(0.691221298772308,0.,0.722643145766653));
#31868=DIRECTION('ref_axis',(0.722643145766653,0.,-0.691221298772308));
#31869=DIRECTION('',(0.,1.,0.));
#31870=DIRECTION('center_axis',(-0.161938741065865,0.,0.986800812799626));
#31871=DIRECTION('ref_axis',(0.986800812799626,0.,0.161938741065865));
#31872=DIRECTION('',(0.,1.,0.));
#31873=DIRECTION('center_axis',(-0.220607484589183,0.,0.975362669853236));
#31874=DIRECTION('ref_axis',(0.975362669853236,0.,0.220607484589183));
#31875=DIRECTION('',(0.,1.,0.));
#31876=DIRECTION('center_axis',(-0.28181631667558,0.,0.959468375536896));
#31877=DIRECTION('ref_axis',(0.959468375536896,0.,0.28181631667558));
#31878=DIRECTION('',(0.,1.,0.));
#31879=DIRECTION('center_axis',(-0.346203891732262,0.,0.938159296361464));
#31880=DIRECTION('ref_axis',(0.938159296361463,0.,0.346203891732262));
#31881=DIRECTION('',(0.,1.,0.));
#31882=DIRECTION('center_axis',(-0.414834765185062,0.,0.909896762052627));
#31883=DIRECTION('ref_axis',(0.909896762052626,0.,0.414834765185062));
#31884=DIRECTION('',(0.,1.,0.));
#31885=DIRECTION('center_axis',(-0.489693230637852,0.,0.87189479862393));
#31886=DIRECTION('ref_axis',(0.87189479862393,0.,0.489693230637852));
#31887=DIRECTION('',(0.,1.,0.));
#31888=DIRECTION('center_axis',(-0.575333541465516,0.,0.817918893329129));
#31889=DIRECTION('ref_axis',(0.817918893329129,0.,0.575333541465516));
#31890=DIRECTION('center_axis',(0.543809648975832,0.,0.839208594856358));
#31891=DIRECTION('ref_axis',(0.839208594856358,0.,-0.543809648975832));
#31892=DIRECTION('center_axis',(0.,1.,0.));
#31893=DIRECTION('ref_axis',(0.,0.,1.));
#31894=DIRECTION('',(0.,-1.,0.));
#31895=DIRECTION('center_axis',(0.,1.,0.));
#31896=DIRECTION('ref_axis',(1.,0.,0.));
#31897=DIRECTION('center_axis',(0.,-1.,0.));
#31898=DIRECTION('ref_axis',(0.,0.,-1.));
#31899=DIRECTION('center_axis',(0.,1.,0.));
#31900=DIRECTION('ref_axis',(0.,0.,1.));
#31901=DIRECTION('center_axis',(0.,1.,0.));
#31902=DIRECTION('ref_axis',(1.,0.,0.));
#31903=DIRECTION('',(0.,-1.,0.));
#31904=DIRECTION('center_axis',(0.,1.,0.));
#31905=DIRECTION('ref_axis',(0.,0.,1.));
#31906=DIRECTION('axis',(0.,0.,1.));
#31907=DIRECTION('refdir',(1.,0.,0.));
#31908=DIRECTION('center_axis',(0.,0.,1.));
#31909=DIRECTION('ref_axis',(-1.,0.,0.));
#31910=DIRECTION('',(-1.,0.,0.));
#31911=DIRECTION('',(0.,-1.,0.));
#31912=DIRECTION('',(-1.,0.,0.));
#31913=DIRECTION('',(0.,-1.,0.));
#31914=DIRECTION('center_axis',(1.,0.,0.));
#31915=DIRECTION('ref_axis',(0.,0.,1.));
#31916=DIRECTION('',(0.,0.,1.));
#31917=DIRECTION('',(0.,-1.,0.));
#31918=DIRECTION('',(0.,0.,1.));
#31919=DIRECTION('center_axis',(0.,0.,-1.));
#31920=DIRECTION('ref_axis',(1.,0.,0.));
#31921=DIRECTION('',(1.,0.,0.));
#31922=DIRECTION('',(0.,-1.,0.));
#31923=DIRECTION('',(1.,0.,0.));
#31924=DIRECTION('center_axis',(-1.,0.,0.));
#31925=DIRECTION('ref_axis',(0.,0.,-1.));
#31926=DIRECTION('',(0.,0.,-1.));
#31927=DIRECTION('',(0.,0.,-1.));
#31928=DIRECTION('center_axis',(0.,-1.,0.));
#31929=DIRECTION('ref_axis',(0.,0.,-1.));
#31930=DIRECTION('center_axis',(-1.,0.,0.));
#31931=DIRECTION('ref_axis',(0.,0.,-1.));
#31932=DIRECTION('',(0.,0.,-1.));
#31933=DIRECTION('',(0.,-1.,0.));
#31934=DIRECTION('',(0.,0.,-1.));
#31935=DIRECTION('',(0.,-1.,0.));
#31936=DIRECTION('center_axis',(0.,0.,1.));
#31937=DIRECTION('ref_axis',(-1.,0.,0.));
#31938=DIRECTION('',(-1.,0.,0.));
#31939=DIRECTION('',(0.,-1.,0.));
#31940=DIRECTION('',(-1.,0.,0.));
#31941=DIRECTION('center_axis',(1.,0.,0.));
#31942=DIRECTION('ref_axis',(0.,0.,1.));
#31943=DIRECTION('',(0.,0.,1.));
#31944=DIRECTION('',(0.,-1.,0.));
#31945=DIRECTION('',(0.,0.,1.));
#31946=DIRECTION('center_axis',(0.,0.,-1.));
#31947=DIRECTION('ref_axis',(1.,0.,0.));
#31948=DIRECTION('',(1.,0.,0.));
#31949=DIRECTION('',(1.,0.,0.));
#31950=DIRECTION('center_axis',(0.,-1.,0.));
#31951=DIRECTION('ref_axis',(0.,0.,-1.));
#31952=DIRECTION('center_axis',(0.,1.,0.));
#31953=DIRECTION('ref_axis',(1.,0.,0.));
#31954=DIRECTION('center_axis',(0.,1.,0.));
#31955=DIRECTION('ref_axis',(1.,0.,0.));
#31956=DIRECTION('',(0.,1.,0.));
#31957=DIRECTION('center_axis',(0.,-1.,0.));
#31958=DIRECTION('ref_axis',(1.,0.,0.));
#31959=DIRECTION('center_axis',(0.,1.,0.));
#31960=DIRECTION('ref_axis',(1.,0.,0.));
#31961=DIRECTION('center_axis',(0.,1.,0.));
#31962=DIRECTION('ref_axis',(1.,0.,0.));
#31963=DIRECTION('',(0.,1.,0.));
#31964=DIRECTION('center_axis',(0.,-1.,0.));
#31965=DIRECTION('ref_axis',(1.,0.,0.));
#31966=DIRECTION('center_axis',(0.,1.,0.));
#31967=DIRECTION('ref_axis',(-1.83697019872103E-16,0.,1.));
#31968=DIRECTION('center_axis',(0.,1.,0.));
#31969=DIRECTION('ref_axis',(1.,0.,0.));
#31970=DIRECTION('',(0.,1.,0.));
#31971=DIRECTION('center_axis',(0.,1.,0.));
#31972=DIRECTION('ref_axis',(1.,0.,0.));
#31973=DIRECTION('',(0.,1.,0.));
#31974=DIRECTION('center_axis',(0.,1.,0.));
#31975=DIRECTION('ref_axis',(-1.60812264967664E-16,0.,-1.));
#31976=DIRECTION('center_axis',(0.,1.,0.));
#31977=DIRECTION('ref_axis',(1.,0.,0.));
#31978=DIRECTION('center_axis',(0.,1.,0.));
#31979=DIRECTION('ref_axis',(1.,0.,0.));
#31980=DIRECTION('center_axis',(0.,1.,0.));
#31981=DIRECTION('ref_axis',(1.,0.,0.));
#31982=DIRECTION('center_axis',(0.,1.,0.));
#31983=DIRECTION('ref_axis',(1.,0.,0.));
#31984=DIRECTION('axis',(0.,0.,1.));
#31985=DIRECTION('refdir',(1.,0.,0.));
#31986=DIRECTION('center_axis',(1.,0.,-3.89588521716247E-15));
#31987=DIRECTION('ref_axis',(0.,-1.,-3.13402942782487E-17));
#31988=DIRECTION('center_axis',(-1.,0.,0.));
#31989=DIRECTION('ref_axis',(0.,-1.,-6.12323399573677E-17));
#31990=DIRECTION('center_axis',(-1.,0.,0.));
#31991=DIRECTION('ref_axis',(0.,-1.,-6.12323399573677E-17));
#31992=DIRECTION('',(-0.322006219579217,-0.946737553154147,1.10888632576264E-15));
#31993=DIRECTION('center_axis',(1.,0.,0.));
#31994=DIRECTION('ref_axis',(0.,-1.,0.));
#31995=DIRECTION('center_axis',(-1.,0.,0.));
#31996=DIRECTION('ref_axis',(0.,0.,1.));
#31997=DIRECTION('center_axis',(1.,0.,0.));
#31998=DIRECTION('ref_axis',(0.,0.,-1.));
#31999=DIRECTION('center_axis',(1.,0.,0.));
#32000=DIRECTION('ref_axis',(0.,1.,0.));
#32001=DIRECTION('center_axis',(1.,0.,0.));
#32002=DIRECTION('ref_axis',(0.,0.,-1.));
#32003=DIRECTION('',(-0.609710760849692,0.7926239891046,9.70684431184355E-17));
#32004=DIRECTION('center_axis',(1.,0.,0.));
#32005=DIRECTION('ref_axis',(0.,1.,0.));
#32006=DIRECTION('center_axis',(1.,0.,0.));
#32007=DIRECTION('ref_axis',(0.,0.,-1.));
#32008=DIRECTION('',(-1.,0.,0.));
#32009=DIRECTION('center_axis',(-1.,0.,0.));
#32010=DIRECTION('ref_axis',(0.,0.,1.));
#32011=DIRECTION('center_axis',(1.,0.,0.));
#32012=DIRECTION('ref_axis',(0.,0.,-1.));
#32013=DIRECTION('center_axis',(1.,0.,0.));
#32014=DIRECTION('ref_axis',(0.,1.,0.));
#32015=DIRECTION('center_axis',(1.,0.,0.));
#32016=DIRECTION('ref_axis',(0.,0.,-1.));
#32017=DIRECTION('',(-1.,0.,0.));
#32018=DIRECTION('center_axis',(1.,0.,0.));
#32019=DIRECTION('ref_axis',(0.,0.,-1.));
#32020=DIRECTION('center_axis',(1.,0.,0.));
#32021=DIRECTION('ref_axis',(0.,0.,-1.));
#32022=DIRECTION('center_axis',(1.,0.,0.));
#32023=DIRECTION('ref_axis',(0.,1.,0.));
#32024=DIRECTION('',(-1.,0.,0.));
#32025=DIRECTION('center_axis',(1.,0.,0.));
#32026=DIRECTION('ref_axis',(0.,0.,-1.));
#32027=DIRECTION('center_axis',(1.,0.,0.));
#32028=DIRECTION('ref_axis',(0.,0.,-1.));
#32029=DIRECTION('center_axis',(1.,0.,0.));
#32030=DIRECTION('ref_axis',(0.,0.,-1.));
#32031=DIRECTION('center_axis',(1.,0.,0.));
#32032=DIRECTION('ref_axis',(0.,1.,0.));
#32033=DIRECTION('',(-0.662716862978517,0.748870055165724,9.17101316036005E-17));
#32034=DIRECTION('axis',(0.,0.,1.));
#32035=DIRECTION('refdir',(1.,0.,0.));
#32036=DIRECTION('center_axis',(0.707106781186548,0.707106781186547,0.));
#32037=DIRECTION('ref_axis',(0.,0.,-1.));
#32038=DIRECTION('',(0.,0.,1.));
#32039=DIRECTION('center_axis',(0.707106781186548,0.707106781186547,0.));
#32040=DIRECTION('ref_axis',(0.707106781186547,-0.707106781186548,5.34045053974073E-17));
#32041=DIRECTION('',(0.,0.,-1.));
#32042=DIRECTION('center_axis',(1.,0.,0.));
#32043=DIRECTION('ref_axis',(0.,0.245901639344262,-0.969294786825868));
#32044=DIRECTION('center_axis',(-1.,0.,0.));
#32045=DIRECTION('ref_axis',(0.,0.245901639344262,-0.969294786825868));
#32046=DIRECTION('center_axis',(1.,0.,0.));
#32047=DIRECTION('ref_axis',(0.,0.245901639344262,-0.969294786825868));
#32048=DIRECTION('center_axis',(0.707106781186548,-0.707106781186547,0.));
#32049=DIRECTION('ref_axis',(0.,0.,-1.));
#32050=DIRECTION('',(0.,0.,1.));
#32051=DIRECTION('center_axis',(0.707106781186548,-0.707106781186547,0.));
#32052=DIRECTION('ref_axis',(-0.707106781186547,-0.707106781186548,5.34045053974073E-17));
#32053=DIRECTION('',(0.,0.,-1.));
#32054=DIRECTION('center_axis',(0.,1.,0.));
#32055=DIRECTION('ref_axis',(0.,0.,1.));
#32056=DIRECTION('',(1.,0.,0.));
#32057=DIRECTION('',(0.,0.,-1.));
#32058=DIRECTION('',(1.,0.,0.));
#32059=DIRECTION('center_axis',(1.,0.,0.));
#32060=DIRECTION('ref_axis',(0.,-1.36502830896536E-16,-1.));
#32061=DIRECTION('',(1.,0.,0.));
#32062=DIRECTION('center_axis',(1.,0.,0.));
#32063=DIRECTION('ref_axis',(0.,0.245901639344262,-0.969294786825868));
#32064=DIRECTION('center_axis',(0.,-1.,0.));
#32065=DIRECTION('ref_axis',(0.,0.,-1.));
#32066=DIRECTION('',(1.,0.,0.));
#32067=DIRECTION('',(0.,0.,1.));
#32068=DIRECTION('center_axis',(-0.707106781186548,-0.707106781186547,0.));
#32069=DIRECTION('ref_axis',(0.,0.,1.));
#32070=DIRECTION('center_axis',(-0.707106781186548,-0.707106781186547,0.));
#32071=DIRECTION('ref_axis',(0.707106781186547,-0.707106781186548,5.34045053974073E-17));
#32072=DIRECTION('',(0.,0.,-1.));
#32073=DIRECTION('center_axis',(-1.,0.,0.));
#32074=DIRECTION('ref_axis',(0.,0.245901639344262,-0.969294786825868));
#32075=DIRECTION('center_axis',(-1.,0.,0.));
#32076=DIRECTION('ref_axis',(0.,0.245901639344262,-0.969294786825868));
#32077=DIRECTION('center_axis',(-0.707106781186548,0.707106781186547,0.));
#32078=DIRECTION('ref_axis',(0.,0.,1.));
#32079=DIRECTION('',(0.,0.,1.));
#32080=DIRECTION('center_axis',(-0.707106781186548,0.707106781186547,0.));
#32081=DIRECTION('ref_axis',(-0.707106781186547,-0.707106781186548,5.34045053974073E-17));
#32082=DIRECTION('center_axis',(1.,0.,0.));
#32083=DIRECTION('ref_axis',(0.,0.,-1.));
#32084=DIRECTION('center_axis',(1.,0.,0.));
#32085=DIRECTION('ref_axis',(0.,-0.204081632653062,0.978953873894813));
#32086=DIRECTION('center_axis',(-1.,0.,0.));
#32087=DIRECTION('ref_axis',(0.,0.,-1.));
#32088=DIRECTION('center_axis',(-1.,0.,0.));
#32089=DIRECTION('ref_axis',(0.,0.,-1.));
#32090=DIRECTION('center_axis',(1.,0.,0.));
#32091=DIRECTION('ref_axis',(0.,9.44067197810507E-16,-1.));
#32092=DIRECTION('center_axis',(1.,0.,0.));
#32093=DIRECTION('ref_axis',(0.,-0.204081632653062,0.978953873894813));
#32094=DIRECTION('center_axis',(-1.,0.,0.));
#32095=DIRECTION('ref_axis',(0.,0.,-1.));
#32096=DIRECTION('',(0.707106781186547,-8.65956056235494E-17,-0.707106781186548));
#32097=DIRECTION('center_axis',(1.,0.,0.));
#32098=DIRECTION('ref_axis',(0.,0.,-1.));
#32099=DIRECTION('center_axis',(1.,0.,0.));
#32100=DIRECTION('ref_axis',(0.,0.,-1.));
#32101=DIRECTION('',(1.,0.,0.));
#32102=DIRECTION('center_axis',(-1.,0.,0.));
#32103=DIRECTION('ref_axis',(0.,0.,-1.));
#32104=DIRECTION('center_axis',(1.,0.,0.));
#32105=DIRECTION('ref_axis',(0.,0.,-1.));
#32106=DIRECTION('center_axis',(1.,0.,0.));
#32107=DIRECTION('ref_axis',(0.,0.,-1.));
#32108=DIRECTION('',(-0.707106781186547,8.65956056235494E-17,-0.707106781186548));
#32109=DIRECTION('center_axis',(1.,0.,0.));
#32110=DIRECTION('ref_axis',(0.,0.,-1.));
#32111=DIRECTION('center_axis',(1.,0.,0.));
#32112=DIRECTION('ref_axis',(0.,0.,-1.));
#32113=DIRECTION('center_axis',(-1.,0.,0.));
#32114=DIRECTION('ref_axis',(0.,0.,-1.));
#32115=DIRECTION('',(0.707106781186547,-8.65956056235494E-17,-0.707106781186548));
#32116=DIRECTION('center_axis',(1.,0.,0.));
#32117=DIRECTION('ref_axis',(0.,0.,-1.));
#32118=DIRECTION('center_axis',(1.,0.,0.));
#32119=DIRECTION('ref_axis',(0.,0.,-1.));
#32120=DIRECTION('',(1.,0.,0.));
#32121=DIRECTION('center_axis',(-1.,0.,0.));
#32122=DIRECTION('ref_axis',(0.,0.,-1.));
#32123=DIRECTION('center_axis',(1.,0.,0.));
#32124=DIRECTION('ref_axis',(0.,0.,-1.));
#32125=DIRECTION('',(-0.707106781186547,8.65956056235494E-17,-0.707106781186548));
#32126=DIRECTION('axis',(0.,0.,1.));
#32127=DIRECTION('refdir',(1.,0.,0.));
#32128=DIRECTION('center_axis',(0.707106781186548,-0.707106781186548,0.));
#32129=DIRECTION('ref_axis',(0.,0.,-1.));
#32130=DIRECTION('',(-0.577350269189626,-0.577350269189626,-0.577350269189626));
#32131=DIRECTION('',(0.,0.,-1.));
#32132=DIRECTION('',(0.577350269189626,0.577350269189626,-0.577350269189626));
#32133=DIRECTION('',(0.577350269189626,0.577350269189626,0.577350269189626));
#32134=DIRECTION('',(0.,0.,1.));
#32135=DIRECTION('',(-0.577350269189627,-0.577350269189627,0.577350269189624));
#32136=DIRECTION('center_axis',(1.,0.,0.));
#32137=DIRECTION('ref_axis',(0.,0.,-1.));
#32138=DIRECTION('',(0.,-1.,0.));
#32139=DIRECTION('',(0.,0.,-1.));
#32140=DIRECTION('',(0.,1.,0.));
#32141=DIRECTION('center_axis',(0.707106781186548,0.,-0.707106781186548));
#32142=DIRECTION('ref_axis',(-0.707106781186548,0.,-0.707106781186548));
#32143=DIRECTION('',(0.577350269189626,-0.577350269189626,0.577350269189626));
#32144=DIRECTION('',(0.,1.,0.));
#32145=DIRECTION('',(-0.577350269189624,-0.57735026918963,-0.577350269189624));
#32146=DIRECTION('',(-0.577350269189624,0.57735026918963,-0.577350269189624));
#32147=DIRECTION('center_axis',(0.,-0.707106781186548,-0.707106781186548));
#32148=DIRECTION('ref_axis',(-1.,0.,0.));
#32149=DIRECTION('',(-1.,0.,0.));
#32150=DIRECTION('',(0.577350269189626,-0.577350269189626,0.577350269189626));
#32151=DIRECTION('',(0.577350269189628,0.577350269189625,-0.577350269189625));
#32152=DIRECTION('',(1.,0.,0.));
#32153=DIRECTION('center_axis',(-0.707106781186548,-0.707106781186548,0.));
#32154=DIRECTION('ref_axis',(0.,0.,1.));
#32155=DIRECTION('',(0.,0.,1.));
#32156=DIRECTION('',(-0.577350269189626,0.577350269189626,0.577350269189626));
#32157=DIRECTION('',(-0.577350269189626,0.577350269189626,-0.577350269189626));
#32158=DIRECTION('',(0.,0.,-1.));
#32159=DIRECTION('',(0.577350269189627,-0.577350269189627,-0.577350269189624));
#32160=DIRECTION('center_axis',(-1.,0.,0.));
#32161=DIRECTION('ref_axis',(0.,0.,1.));
#32162=DIRECTION('',(0.,-1.,0.));
#32163=DIRECTION('',(0.,0.,1.));
#32164=DIRECTION('',(0.,1.,0.));
#32165=DIRECTION('center_axis',(-0.707106781186548,0.,0.707106781186548));
#32166=DIRECTION('ref_axis',(0.707106781186548,0.,0.707106781186548));
#32167=DIRECTION('',(-0.577350269189626,-0.577350269189626,-0.577350269189626));
#32168=DIRECTION('',(0.,1.,0.));
#32169=DIRECTION('',(0.577350269189624,-0.57735026918963,0.577350269189624));
#32170=DIRECTION('',(0.577350269189624,0.57735026918963,0.577350269189624));
#32171=DIRECTION('center_axis',(0.,-0.707106781186548,0.707106781186548));
#32172=DIRECTION('ref_axis',(1.,0.,0.));
#32173=DIRECTION('',(-0.577350269189628,0.577350269189625,0.577350269189625));
#32174=DIRECTION('',(-1.,0.,0.));
#32175=DIRECTION('',(1.,0.,0.));
#32176=DIRECTION('center_axis',(0.,0.,-1.));
#32177=DIRECTION('ref_axis',(-1.,0.,0.));
#32178=DIRECTION('',(0.,-1.,0.));
#32179=DIRECTION('',(-1.,0.,0.));
#32180=DIRECTION('center_axis',(-0.707106781186551,0.707106781186544,0.));
#32181=DIRECTION('ref_axis',(0.,0.,1.));
#32182=DIRECTION('',(0.577350269189624,0.57735026918963,-0.577350269189624));
#32183=DIRECTION('',(0.,0.,-1.));
#32184=DIRECTION('',(-0.577350269189624,-0.57735026918963,-0.577350269189624));
#32185=DIRECTION('',(-0.577350269189625,-0.577350269189631,0.577350269189622));
#32186=DIRECTION('center_axis',(0.,0.707106781186544,-0.707106781186551));
#32187=DIRECTION('ref_axis',(-1.,0.,0.));
#32188=DIRECTION('',(1.,0.,0.));
#32189=DIRECTION('',(0.577350269189624,-0.57735026918963,-0.577350269189624));
#32190=DIRECTION('',(-0.577350269189625,0.577350269189629,0.577350269189623));
#32191=DIRECTION('center_axis',(0.,1.,0.));
#32192=DIRECTION('ref_axis',(0.,0.,1.));
#32193=DIRECTION('',(-1.,0.,0.));
#32194=DIRECTION('',(0.,0.,1.));
#32195=DIRECTION('center_axis',(0.,0.707106781186544,0.707106781186551));
#32196=DIRECTION('ref_axis',(1.,0.,0.));
#32197=DIRECTION('',(1.,0.,0.));
#32198=DIRECTION('',(0.577350269189625,0.577350269189629,-0.577350269189623));
#32199=DIRECTION('',(0.577350269189624,-0.57735026918963,0.577350269189624));
#32200=DIRECTION('center_axis',(0.707106781186551,0.707106781186544,0.));
#32201=DIRECTION('ref_axis',(0.,0.,-1.));
#32202=DIRECTION('',(0.577350269189625,-0.577350269189631,-0.577350269189622));
#32203=DIRECTION('center_axis',(0.707106781186546,0.,0.707106781186549));
#32204=DIRECTION('ref_axis',(0.707106781186549,0.,-0.707106781186546));
#32205=DIRECTION('',(0.,-1.,0.));
#32206=DIRECTION('center_axis',(0.,0.,1.));
#32207=DIRECTION('ref_axis',(1.,0.,0.));
#32208=DIRECTION('center_axis',(-0.707106781186546,0.,-0.707106781186549));
#32209=DIRECTION('ref_axis',(-0.707106781186549,0.,0.707106781186546));
#32210=DIRECTION('center_axis',(0.,1.,0.));
#32211=DIRECTION('ref_axis',(1.,0.,0.));
#32212=DIRECTION('axis',(0.,0.,1.));
#32213=DIRECTION('refdir',(1.,0.,0.));
#32214=DIRECTION('center_axis',(0.,1.,0.));
#32215=DIRECTION('ref_axis',(0.,0.,1.));
#32216=DIRECTION('center_axis',(2.44929359829471E-16,0.,-1.));
#32217=DIRECTION('ref_axis',(2.22044604925031E-16,1.,5.43852429378756E-32));
#32218=DIRECTION('center_axis',(2.44929359829471E-16,0.,-1.));
#32219=DIRECTION('ref_axis',(2.22044604925031E-16,1.,5.43852429378756E-32));
#32220=DIRECTION('center_axis',(0.,-1.,0.));
#32221=DIRECTION('ref_axis',(0.,0.,1.));
#32222=DIRECTION('center_axis',(-1.22464679914735E-16,0.,1.));
#32223=DIRECTION('ref_axis',(-2.22044604925031E-16,1.,-2.71926214689378E-32));
#32224=DIRECTION('center_axis',(-1.22464679914735E-16,0.,1.));
#32225=DIRECTION('ref_axis',(-2.22044604925031E-16,1.,-2.71926214689378E-32));
#32226=DIRECTION('center_axis',(0.,0.,1.));
#32227=DIRECTION('ref_axis',(-2.22044604925031E-16,1.,0.));
#32228=DIRECTION('',(0.,0.,-1.));
#32229=DIRECTION('center_axis',(-1.22464679914735E-16,0.,1.));
#32230=DIRECTION('ref_axis',(-2.22044604925031E-16,1.,-2.71926214689378E-32));
#32231=DIRECTION('center_axis',(-1.22464679914735E-16,0.,1.));
#32232=DIRECTION('ref_axis',(-2.22044604925031E-16,1.,-2.71926214689378E-32));
#32233=DIRECTION('center_axis',(0.,1.,0.));
#32234=DIRECTION('ref_axis',(-1.22464679914735E-16,0.,-1.));
#32235=DIRECTION('center_axis',(0.,-1.,0.));
#32236=DIRECTION('ref_axis',(-1.22464679914735E-16,0.,-1.));
#32237=DIRECTION('center_axis',(0.,0.,-1.));
#32238=DIRECTION('ref_axis',(2.22044604925031E-16,1.,0.));
#32239=DIRECTION('center_axis',(0.,0.,-1.));
#32240=DIRECTION('ref_axis',(2.22044604925031E-16,1.,0.));
#32241=DIRECTION('center_axis',(0.,0.,-1.));
#32242=DIRECTION('ref_axis',(2.22044604925031E-16,1.,0.));
#32243=DIRECTION('',(0.,0.,1.));
#32244=DIRECTION('axis',(0.,0.,1.));
#32245=DIRECTION('refdir',(1.,0.,0.));
#32246=DIRECTION('center_axis',(-0.54775000523585,5.84175495892749E-17,
-0.836642057133232));
#32247=DIRECTION('ref_axis',(-0.836642057133232,0.,0.54775000523585));
#32248=DIRECTION('',(0.,1.,1.28197512425571E-15));
#32249=DIRECTION('',(0.677497944020808,-0.586730430533752,-0.443558268701257));
#32250=DIRECTION('',(-0.677497944020811,-0.586730430533747,0.443558268701259));
#32251=DIRECTION('center_axis',(-0.54775000523585,0.724553275351851,-0.418321028566616));
#32252=DIRECTION('ref_axis',(-0.606949534647158,0.,0.79474037420506));
#32253=DIRECTION('',(0.677497944020812,0.0907675134870681,-0.729902592366233));
#32254=DIRECTION('',(-0.677497944020808,-0.677497944020809,-0.286344323664981));
#32255=DIRECTION('',(0.,0.499999999999999,0.866025403784439));
#32256=DIRECTION('center_axis',(-0.547750005235851,-0.72455327535185,-0.418321028566615));
#32257=DIRECTION('ref_axis',(-0.606949534647157,0.,0.79474037420506));
#32258=DIRECTION('',(0.,0.499999999999999,-0.866025403784439));
#32259=DIRECTION('',(0.677497944020809,-0.677497944020809,0.286344323664978));
#32260=DIRECTION('',(-0.677497944020809,0.0907675134870617,0.729902592366237));
#32261=DIRECTION('center_axis',(-0.54775000523585,0.724553275351851,0.418321028566614));
#32262=DIRECTION('ref_axis',(0.606949534647157,0.,0.794740374205061));
#32263=DIRECTION('',(0.,-0.5,0.866025403784439));
#32264=DIRECTION('',(0.677497944020808,0.677497944020808,-0.286344323664982));
#32265=DIRECTION('',(-0.677497944020809,-0.0907675134870617,-0.729902592366237));
#32266=DIRECTION('center_axis',(-0.707106781186548,0.707106781186547,-2.33098278087517E-16));
#32267=DIRECTION('ref_axis',(-3.29650746237182E-16,0.,1.));
#32268=DIRECTION('',(0.,-3.29650746237182E-16,-1.));
#32269=DIRECTION('',(0.,3.29650746237182E-16,1.));
#32270=DIRECTION('center_axis',(-0.547750005235851,-0.724553275351851,0.418321028566615));
#32271=DIRECTION('ref_axis',(0.606949534647157,0.,0.79474037420506));
#32272=DIRECTION('',(0.,-0.5,-0.866025403784439));
#32273=DIRECTION('',(0.677497944020811,-0.0907675134870634,0.729902592366235));
#32274=DIRECTION('',(-0.677497944020808,0.677497944020809,0.286344323664979));
#32275=DIRECTION('center_axis',(-0.54775000523585,-1.10993344219622E-15,
0.836642057133232));
#32276=DIRECTION('ref_axis',(0.836642057133232,0.,0.54775000523585));
#32277=DIRECTION('',(0.,-1.,-2.56395024851142E-15));
#32278=DIRECTION('',(0.677497944020809,0.586730430533748,0.44355826870126));
#32279=DIRECTION('',(-0.67749794402081,0.586730430533748,-0.443558268701259));
#32280=DIRECTION('center_axis',(-0.707106781186548,0.353553390593274,0.612372435695794));
#32281=DIRECTION('ref_axis',(0.654653670707977,0.,0.755928946018455));
#32282=DIRECTION('',(0.,0.866025403784439,-0.5));
#32283=DIRECTION('',(0.,-0.866025403784439,0.5));
#32284=DIRECTION('center_axis',(-0.707106781186547,-0.353553390593274,0.612372435695795));
#32285=DIRECTION('ref_axis',(0.654653670707978,0.,0.755928946018454));
#32286=DIRECTION('',(0.,0.866025403784439,0.5));
#32287=DIRECTION('',(0.,-0.866025403784439,-0.5));
#32288=DIRECTION('center_axis',(0.,-2.56395024851142E-15,1.));
#32289=DIRECTION('ref_axis',(1.,0.,0.));
#32290=DIRECTION('',(-1.,0.,0.));
#32291=DIRECTION('',(1.,0.,0.));
#32292=DIRECTION('center_axis',(-0.707106781186548,-0.707106781186547,0.));
#32293=DIRECTION('ref_axis',(0.,0.,1.));
#32294=DIRECTION('',(0.,0.,1.));
#32295=DIRECTION('',(0.,0.,-1.));
#32296=DIRECTION('center_axis',(0.,-0.866025403784439,0.5));
#32297=DIRECTION('ref_axis',(0.,-0.5,-0.866025403784439));
#32298=DIRECTION('',(-1.,0.,0.));
#32299=DIRECTION('',(1.,0.,0.));
#32300=DIRECTION('center_axis',(0.,0.866025403784439,0.5));
#32301=DIRECTION('ref_axis',(0.,-0.5,0.866025403784439));
#32302=DIRECTION('',(-1.,0.,0.));
#32303=DIRECTION('',(1.,0.,0.));
#32304=DIRECTION('center_axis',(-0.707106781186547,-0.353553390593274,-0.612372435695794));
#32305=DIRECTION('ref_axis',(-0.654653670707977,0.,0.755928946018454));
#32306=DIRECTION('',(0.,-0.866025403784439,0.5));
#32307=DIRECTION('',(0.,0.866025403784439,-0.5));
#32308=DIRECTION('center_axis',(0.,-0.866025403784439,-0.5));
#32309=DIRECTION('ref_axis',(0.,0.5,-0.866025403784439));
#32310=DIRECTION('',(-1.,0.,0.));
#32311=DIRECTION('',(1.,0.,0.));
#32312=DIRECTION('center_axis',(0.,0.866025403784439,-0.499999999999999));
#32313=DIRECTION('ref_axis',(0.,0.499999999999999,0.866025403784439));
#32314=DIRECTION('',(-1.,0.,0.));
#32315=DIRECTION('',(1.,0.,0.));
#32316=DIRECTION('center_axis',(-0.707106781186546,0.353553390593275,-0.612372435695796));
#32317=DIRECTION('ref_axis',(-0.654653670707979,0.,0.755928946018453));
#32318=DIRECTION('',(0.,-0.866025403784439,-0.5));
#32319=DIRECTION('',(0.,0.866025403784439,0.5));
#32320=DIRECTION('center_axis',(0.,1.28197512425571E-15,-1.));
#32321=DIRECTION('ref_axis',(-1.,0.,0.));
#32322=DIRECTION('',(-1.,0.,0.));
#32323=DIRECTION('',(1.,0.,0.));
#32324=DIRECTION('center_axis',(0.,-0.5,0.866025403784439));
#32325=DIRECTION('ref_axis',(0.,-0.866025403784439,-0.5));
#32326=DIRECTION('center_axis',(0.,-1.,0.));
#32327=DIRECTION('ref_axis',(0.,0.,-1.));
#32328=DIRECTION('center_axis',(0.,-0.5,-0.866025403784439));
#32329=DIRECTION('ref_axis',(0.,0.866025403784439,-0.5));
#32330=DIRECTION('center_axis',(1.,0.,0.));
#32331=DIRECTION('ref_axis',(0.,0.,-1.));
#32332=DIRECTION('center_axis',(1.,0.,0.));
#32333=DIRECTION('ref_axis',(0.,0.,-1.));
#32334=DIRECTION('center_axis',(0.707106781186547,0.353553390593274,0.612372435695795));
#32335=DIRECTION('ref_axis',(0.654653670707978,0.,-0.755928946018454));
#32336=DIRECTION('',(0.,0.866025403784439,-0.5));
#32337=DIRECTION('',(-0.654653670707977,-4.69765578524213E-16,0.755928946018454));
#32338=DIRECTION('',(0.,-0.866025403784439,0.5));
#32339=DIRECTION('',(-0.654653670707978,0.654653670707977,0.377964473009227));
#32340=DIRECTION('center_axis',(0.707106781186548,-0.353553390593273,0.612372435695795));
#32341=DIRECTION('ref_axis',(0.654653670707977,0.,-0.755928946018455));
#32342=DIRECTION('',(0.,0.866025403784439,0.5));
#32343=DIRECTION('',(-0.654653670707977,-0.654653670707976,0.377964473009229));
#32344=DIRECTION('',(0.,-0.866025403784439,-0.5));
#32345=DIRECTION('center_axis',(0.707106781186547,-0.353553390593274,-0.612372435695795));
#32346=DIRECTION('ref_axis',(-0.654653670707978,0.,-0.755928946018454));
#32347=DIRECTION('',(0.,-0.866025403784439,0.5));
#32348=DIRECTION('',(-0.654653670707977,1.00453536761267E-15,-0.755928946018454));
#32349=DIRECTION('',(0.,0.866025403784439,-0.5));
#32350=DIRECTION('',(0.654653670707978,0.654653670707977,0.377964473009227));
#32351=DIRECTION('center_axis',(0.707106781186548,0.353553390593274,-0.612372435695794));
#32352=DIRECTION('ref_axis',(-0.654653670707977,0.,-0.755928946018455));
#32353=DIRECTION('',(0.,0.866025403784439,0.5));
#32354=DIRECTION('',(0.,-0.866025403784439,-0.5));
#32355=DIRECTION('',(-0.654653670707977,0.654653670707977,-0.377964473009228));
#32356=DIRECTION('center_axis',(0.707106781186547,-0.707106781186548,2.2662332591842E-16));
#32357=DIRECTION('ref_axis',(3.20493781063928E-16,0.,-1.));
#32358=DIRECTION('',(0.,3.20493781063927E-16,1.));
#32359=DIRECTION('',(0.,-3.20493781063927E-16,-1.));
#32360=DIRECTION('center_axis',(0.707106781186547,0.707106781186548,1.1331166295921E-16));
#32361=DIRECTION('ref_axis',(1.60246890531964E-16,0.,-1.));
#32362=DIRECTION('',(0.,-1.60246890531964E-16,1.));
#32363=DIRECTION('',(0.,1.60246890531964E-16,-1.));
#32364=DIRECTION('center_axis',(0.,0.5,-0.866025403784439));
#32365=DIRECTION('ref_axis',(0.,-0.866025403784439,-0.5));
#32366=DIRECTION('',(-1.,0.,0.));
#32367=DIRECTION('',(0.,-0.866025403784439,-0.5));
#32368=DIRECTION('',(-1.,0.,0.));
#32369=DIRECTION('center_axis',(0.,1.,-3.20493781063927E-16));
#32370=DIRECTION('ref_axis',(0.,-3.20493781063927E-16,-1.));
#32371=DIRECTION('',(-1.,0.,0.));
#32372=DIRECTION('',(0.,-3.20493781063927E-16,-1.));
#32373=DIRECTION('center_axis',(0.,0.5,0.866025403784439));
#32374=DIRECTION('ref_axis',(0.,0.866025403784439,-0.5));
#32375=DIRECTION('',(-1.,0.,0.));
#32376=DIRECTION('',(0.,0.866025403784439,-0.5));
#32377=DIRECTION('center_axis',(1.,0.,0.));
#32378=DIRECTION('ref_axis',(0.,0.,-1.));
#32379=DIRECTION('center_axis',(1.,0.,0.));
#32380=DIRECTION('ref_axis',(0.,1.,0.));
#32381=DIRECTION('center_axis',(0.,-0.5,0.866025403784439));
#32382=DIRECTION('ref_axis',(0.,0.866025403784439,0.5));
#32383=DIRECTION('',(-1.,0.,0.));
#32384=DIRECTION('',(0.,0.866025403784439,0.5));
#32385=DIRECTION('center_axis',(0.,-1.,-1.60246890531964E-16));
#32386=DIRECTION('ref_axis',(0.,-1.60246890531964E-16,1.));
#32387=DIRECTION('',(-1.,0.,0.));
#32388=DIRECTION('',(0.,-1.60246890531964E-16,1.));
#32389=DIRECTION('center_axis',(0.,-0.5,-0.866025403784439));
#32390=DIRECTION('ref_axis',(0.,-0.866025403784439,0.5));
#32391=DIRECTION('',(0.,-0.866025403784439,0.5));
#32392=DIRECTION('center_axis',(-1.,0.,0.));
#32393=DIRECTION('ref_axis',(0.,0.,1.));
#32394=DIRECTION('center_axis',(-1.,0.,0.));
#32395=DIRECTION('ref_axis',(0.,1.,0.));
#32396=DIRECTION('',(0.500011000363013,0.866019052628739,1.06056746080241E-16));
#32397=DIRECTION('center_axis',(0.,0.5,0.866025403784439));
#32398=DIRECTION('ref_axis',(0.,-0.866025403784439,0.5));
#32399=DIRECTION('center_axis',(0.,1.,-3.29650746237182E-16));
#32400=DIRECTION('ref_axis',(0.,3.29650746237182E-16,1.));
#32401=DIRECTION('center_axis',(0.,0.5,-0.866025403784439));
#32402=DIRECTION('ref_axis',(0.,0.866025403784439,0.5));
#32403=DIRECTION('center_axis',(-1.,0.,0.));
#32404=DIRECTION('ref_axis',(0.,0.,1.));
#32405=DIRECTION('center_axis',(1.,0.,0.));
#32406=DIRECTION('ref_axis',(0.,0.,-1.));
#32407=DIRECTION('center_axis',(1.,0.,0.));
#32408=DIRECTION('ref_axis',(0.,1.,0.));
#32409=DIRECTION('center_axis',(1.,0.,0.));
#32410=DIRECTION('ref_axis',(0.,0.,-1.));
#32411=DIRECTION('',(-0.707106781186547,0.707106781186548,8.65956056235493E-17));
#32412=DIRECTION('center_axis',(1.,0.,0.));
#32413=DIRECTION('ref_axis',(0.,1.,0.));
#32414=DIRECTION('center_axis',(1.,0.,0.));
#32415=DIRECTION('ref_axis',(0.,0.,-1.));
#32416=DIRECTION('',(-1.,0.,0.));
#32417=DIRECTION('center_axis',(1.,0.,0.));
#32418=DIRECTION('ref_axis',(0.,0.,-1.));
#32419=DIRECTION('center_axis',(1.,0.,0.));
#32420=DIRECTION('ref_axis',(0.,0.,-1.));
#32421=DIRECTION('center_axis',(1.,0.,0.));
#32422=DIRECTION('ref_axis',(0.,1.,0.));
#32423=DIRECTION('',(-1.,0.,0.));
#32424=DIRECTION('axis',(0.,0.,1.));
#32425=DIRECTION('refdir',(1.,0.,0.));
#32426=DIRECTION('center_axis',(1.,0.,0.));
#32427=DIRECTION('ref_axis',(0.,1.,0.));
#32428=DIRECTION('center_axis',(1.,0.,0.));
#32429=DIRECTION('ref_axis',(0.,0.,-1.));
#32430=DIRECTION('',(-1.,0.,0.));
#32431=DIRECTION('center_axis',(1.,0.,0.));
#32432=DIRECTION('ref_axis',(0.,0.,-1.));
#32433=DIRECTION('center_axis',(-1.,0.,0.));
#32434=DIRECTION('ref_axis',(0.,0.,1.));
#32435=DIRECTION('center_axis',(1.,0.,0.));
#32436=DIRECTION('ref_axis',(0.,1.,0.));
#32437=DIRECTION('center_axis',(1.,0.,0.));
#32438=DIRECTION('ref_axis',(0.,0.,-1.));
#32439=DIRECTION('center_axis',(-1.,0.,0.));
#32440=DIRECTION('ref_axis',(0.,1.,0.));
#32441=DIRECTION('center_axis',(1.,0.,0.));
#32442=DIRECTION('ref_axis',(0.,1.,0.));
#32443=DIRECTION('center_axis',(1.,0.,0.));
#32444=DIRECTION('ref_axis',(0.,0.,-1.));
#32445=DIRECTION('',(-1.,0.,0.));
#32446=DIRECTION('center_axis',(1.,0.,0.));
#32447=DIRECTION('ref_axis',(0.,1.,0.));
#32448=DIRECTION('center_axis',(1.,0.,0.));
#32449=DIRECTION('ref_axis',(0.,0.,-1.));
#32450=DIRECTION('',(-1.,0.,0.));
#32451=DIRECTION('center_axis',(1.,0.,0.));
#32452=DIRECTION('ref_axis',(0.,0.,-1.));
#32453=DIRECTION('center_axis',(-1.,0.,0.));
#32454=DIRECTION('ref_axis',(0.,0.,1.));
#32455=DIRECTION('center_axis',(1.,0.,0.));
#32456=DIRECTION('ref_axis',(0.,0.,-1.));
#32457=DIRECTION('center_axis',(1.,0.,0.));
#32458=DIRECTION('ref_axis',(0.,1.,0.));
#32459=DIRECTION('center_axis',(1.,0.,0.));
#32460=DIRECTION('ref_axis',(0.,0.,-1.));
#32461=DIRECTION('',(-1.,0.,0.));
#32462=DIRECTION('center_axis',(1.,0.,0.));
#32463=DIRECTION('ref_axis',(0.,0.,-1.));
#32464=DIRECTION('center_axis',(1.,0.,0.));
#32465=DIRECTION('ref_axis',(0.,0.,-1.));
#32466=DIRECTION('center_axis',(1.,0.,0.));
#32467=DIRECTION('ref_axis',(0.,1.,0.));
#32468=DIRECTION('',(-1.,0.,0.));
#32469=DIRECTION('center_axis',(1.,0.,0.));
#32470=DIRECTION('ref_axis',(0.,0.,-1.));
#32471=DIRECTION('center_axis',(-1.,0.,0.));
#32472=DIRECTION('ref_axis',(0.,0.,1.));
#32473=DIRECTION('center_axis',(1.,0.,0.));
#32474=DIRECTION('ref_axis',(0.,1.,0.));
#32475=DIRECTION('',(-1.,0.,0.));
#32476=DIRECTION('center_axis',(1.,0.,0.));
#32477=DIRECTION('ref_axis',(0.,0.,-1.));
#32478=DIRECTION('center_axis',(1.,0.,0.));
#32479=DIRECTION('ref_axis',(0.,0.,-1.));
#32480=DIRECTION('axis',(0.,0.,1.));
#32481=DIRECTION('refdir',(1.,0.,0.));
#32482=DIRECTION('center_axis',(1.,0.,0.));
#32483=DIRECTION('ref_axis',(0.,1.,0.));
#32484=DIRECTION('',(-1.,0.,0.));
#32485=DIRECTION('center_axis',(1.,0.,0.));
#32486=DIRECTION('ref_axis',(0.,1.,0.));
#32487=DIRECTION('center_axis',(1.,0.,0.));
#32488=DIRECTION('ref_axis',(0.,1.,0.));
#32489=DIRECTION('',(-1.,0.,0.));
#32490=DIRECTION('center_axis',(1.,0.,0.));
#32491=DIRECTION('ref_axis',(0.,1.,0.));
#32492=DIRECTION('',(-1.,0.,0.));
#32493=DIRECTION('center_axis',(1.,0.,0.));
#32494=DIRECTION('ref_axis',(0.,1.,0.));
#32495=DIRECTION('',(-1.,0.,0.));
#32496=DIRECTION('center_axis',(1.,0.,0.));
#32497=DIRECTION('ref_axis',(0.,1.,0.));
#32498=DIRECTION('',(-1.,0.,0.));
#32499=DIRECTION('center_axis',(1.,0.,0.));
#32500=DIRECTION('ref_axis',(0.,1.,0.));
#32501=DIRECTION('',(-1.,0.,0.));
#32502=DIRECTION('center_axis',(1.,0.,0.));
#32503=DIRECTION('ref_axis',(0.,1.,0.));
#32504=DIRECTION('',(-1.,0.,0.));
#32505=DIRECTION('center_axis',(1.,0.,0.));
#32506=DIRECTION('ref_axis',(0.,1.,0.));
#32507=DIRECTION('',(-1.,0.,0.));
#32508=DIRECTION('center_axis',(1.,0.,0.));
#32509=DIRECTION('ref_axis',(0.,1.,0.));
#32510=DIRECTION('',(-1.,0.,0.));
#32511=DIRECTION('center_axis',(1.,0.,0.));
#32512=DIRECTION('ref_axis',(0.,1.,0.));
#32513=DIRECTION('',(-1.,0.,0.));
#32514=DIRECTION('center_axis',(1.,0.,0.));
#32515=DIRECTION('ref_axis',(0.,1.,0.));
#32516=DIRECTION('',(-1.,0.,0.));
#32517=DIRECTION('center_axis',(1.,0.,0.));
#32518=DIRECTION('ref_axis',(0.,1.,0.));
#32519=DIRECTION('',(-1.,0.,0.));
#32520=DIRECTION('center_axis',(1.,0.,0.));
#32521=DIRECTION('ref_axis',(0.,1.,0.));
#32522=DIRECTION('',(-1.,0.,0.));
#32523=DIRECTION('center_axis',(1.,0.,0.));
#32524=DIRECTION('ref_axis',(0.,1.,0.));
#32525=DIRECTION('',(-1.,0.,0.));
#32526=DIRECTION('center_axis',(1.,0.,0.));
#32527=DIRECTION('ref_axis',(0.,1.,0.));
#32528=DIRECTION('',(-1.,0.,0.));
#32529=DIRECTION('center_axis',(1.,0.,0.));
#32530=DIRECTION('ref_axis',(0.,1.,0.));
#32531=DIRECTION('',(-1.,0.,0.));
#32532=DIRECTION('center_axis',(1.,0.,0.));
#32533=DIRECTION('ref_axis',(0.,1.,0.));
#32534=DIRECTION('',(-1.,0.,0.));
#32535=DIRECTION('center_axis',(1.,0.,0.));
#32536=DIRECTION('ref_axis',(0.,1.,0.));
#32537=DIRECTION('',(-1.,0.,0.));
#32538=DIRECTION('center_axis',(1.,0.,0.));
#32539=DIRECTION('ref_axis',(0.,1.,0.));
#32540=DIRECTION('',(-1.,0.,0.));
#32541=DIRECTION('center_axis',(1.,0.,0.));
#32542=DIRECTION('ref_axis',(0.,1.,0.));
#32543=DIRECTION('',(-1.,0.,0.));
#32544=DIRECTION('center_axis',(1.,0.,0.));
#32545=DIRECTION('ref_axis',(0.,1.,0.));
#32546=DIRECTION('',(-1.,0.,0.));
#32547=DIRECTION('center_axis',(-1.,0.,0.));
#32548=DIRECTION('ref_axis',(0.,1.,0.));
#32549=DIRECTION('center_axis',(1.,0.,0.));
#32550=DIRECTION('ref_axis',(0.,0.203428885041595,-0.97908972455579));
#32551=DIRECTION('',(1.,0.,0.));
#32552=DIRECTION('center_axis',(1.,0.,0.));
#32553=DIRECTION('ref_axis',(0.,1.,1.07759279891775E-13));
#32554=DIRECTION('center_axis',(1.,0.,0.));
#32555=DIRECTION('ref_axis',(0.,1.,1.07759279891775E-13));
#32556=DIRECTION('',(1.,0.,0.));
#32557=DIRECTION('center_axis',(1.,0.,0.));
#32558=DIRECTION('ref_axis',(0.,1.,1.07759279891775E-13));
#32559=DIRECTION('',(1.,0.,0.));
#32560=DIRECTION('center_axis',(1.,0.,0.));
#32561=DIRECTION('ref_axis',(0.,1.,1.07759279891775E-13));
#32562=DIRECTION('',(1.,0.,0.));
#32563=DIRECTION('center_axis',(1.,0.,0.));
#32564=DIRECTION('ref_axis',(0.,1.,1.07759279891775E-13));
#32565=DIRECTION('',(1.,0.,0.));
#32566=DIRECTION('center_axis',(1.,0.,0.));
#32567=DIRECTION('ref_axis',(0.,1.,1.07759279891775E-13));
#32568=DIRECTION('',(1.,0.,0.));
#32569=DIRECTION('center_axis',(1.,0.,0.));
#32570=DIRECTION('ref_axis',(0.,1.,1.07759279891775E-13));
#32571=DIRECTION('',(1.,0.,0.));
#32572=DIRECTION('center_axis',(1.,0.,0.));
#32573=DIRECTION('ref_axis',(0.,1.,1.07759279891775E-13));
#32574=DIRECTION('',(1.,0.,0.));
#32575=DIRECTION('center_axis',(1.,0.,0.));
#32576=DIRECTION('ref_axis',(0.,1.,1.07759279891775E-13));
#32577=DIRECTION('',(1.,0.,0.));
#32578=DIRECTION('center_axis',(1.,0.,0.));
#32579=DIRECTION('ref_axis',(0.,1.,1.07759279891775E-13));
#32580=DIRECTION('',(1.,0.,0.));
#32581=DIRECTION('center_axis',(1.,0.,0.));
#32582=DIRECTION('ref_axis',(0.,1.,1.07759279891775E-13));
#32583=DIRECTION('',(1.,0.,0.));
#32584=DIRECTION('center_axis',(1.,0.,0.));
#32585=DIRECTION('ref_axis',(0.,1.,1.07759279891775E-13));
#32586=DIRECTION('',(1.,0.,0.));
#32587=DIRECTION('center_axis',(1.,0.,0.));
#32588=DIRECTION('ref_axis',(0.,1.,1.07759279891775E-13));
#32589=DIRECTION('',(1.,0.,0.));
#32590=DIRECTION('center_axis',(1.,0.,0.));
#32591=DIRECTION('ref_axis',(0.,1.,1.07759279891775E-13));
#32592=DIRECTION('',(1.,0.,0.));
#32593=DIRECTION('center_axis',(1.,0.,0.));
#32594=DIRECTION('ref_axis',(0.,1.,1.07759279891775E-13));
#32595=DIRECTION('',(1.,0.,0.));
#32596=DIRECTION('center_axis',(1.,0.,0.));
#32597=DIRECTION('ref_axis',(0.,1.,1.07759279891775E-13));
#32598=DIRECTION('',(1.,0.,0.));
#32599=DIRECTION('center_axis',(1.,0.,0.));
#32600=DIRECTION('ref_axis',(0.,1.,1.07759279891775E-13));
#32601=DIRECTION('',(1.,0.,0.));
#32602=DIRECTION('center_axis',(1.,0.,0.));
#32603=DIRECTION('ref_axis',(0.,1.,1.07759279891775E-13));
#32604=DIRECTION('',(1.,0.,0.));
#32605=DIRECTION('center_axis',(1.,0.,0.));
#32606=DIRECTION('ref_axis',(0.,1.,1.07759279891775E-13));
#32607=DIRECTION('',(1.,0.,0.));
#32608=DIRECTION('center_axis',(1.,0.,0.));
#32609=DIRECTION('ref_axis',(0.,1.,1.07759279891775E-13));
#32610=DIRECTION('',(1.,0.,0.));
#32611=DIRECTION('center_axis',(1.,0.,0.));
#32612=DIRECTION('ref_axis',(0.,0.,-1.));
#32613=DIRECTION('center_axis',(-1.,0.,0.));
#32614=DIRECTION('ref_axis',(0.,1.,0.));
#32615=DIRECTION('center_axis',(1.,0.,0.));
#32616=DIRECTION('ref_axis',(0.,0.,-1.));
#32617=DIRECTION('center_axis',(1.,0.,0.));
#32618=DIRECTION('ref_axis',(0.,1.,0.));
#32619=DIRECTION('center_axis',(1.,0.,0.));
#32620=DIRECTION('ref_axis',(0.,1.,0.));
#32621=DIRECTION('center_axis',(-1.,0.,0.));
#32622=DIRECTION('ref_axis',(0.,1.,1.07759279891775E-13));
#32623=DIRECTION('center_axis',(1.,0.,0.));
#32624=DIRECTION('ref_axis',(0.,0.88891871603891,0.458064969492032));
#32625=DIRECTION('center_axis',(0.,-0.451966109673778,0.892035109009926));
#32626=DIRECTION('ref_axis',(0.,-0.892035109009926,-0.451966109673778));
#32627=DIRECTION('',(-1.,0.,0.));
#32628=DIRECTION('',(0.,-0.892035109009926,-0.451966109673778));
#32629=DIRECTION('',(1.,0.,0.));
#32630=DIRECTION('',(0.,-0.892035109009926,-0.451966109673778));
#32631=DIRECTION('center_axis',(1.,0.,0.));
#32632=DIRECTION('ref_axis',(0.,-0.17364817766693,-0.984807753012208));
#32633=DIRECTION('center_axis',(-1.,0.,0.));
#32634=DIRECTION('ref_axis',(0.,1.,0.));
#32635=DIRECTION('',(0.,0.68365729580961,-0.729803193940867));
#32636=DIRECTION('center_axis',(0.,-0.729803193940867,-0.683657295809611));
#32637=DIRECTION('ref_axis',(0.,0.68365729580961,-0.729803193940867));
#32638=DIRECTION('',(1.,0.,0.));
#32639=DIRECTION('',(0.,0.68365729580961,-0.729803193940867));
#32640=DIRECTION('center_axis',(1.,0.,0.));
#32641=DIRECTION('ref_axis',(0.,-0.17364817766693,-0.984807753012208));
#32642=DIRECTION('center_axis',(1.,0.,0.));
#32643=DIRECTION('ref_axis',(0.,1.,0.));
#32644=DIRECTION('center_axis',(0.,-0.290199457811006,0.956966182624129));
#32645=DIRECTION('ref_axis',(0.,-0.956966182624129,-0.290199457811006));
#32646=DIRECTION('',(-1.,0.,0.));
#32647=DIRECTION('',(0.,-0.956966182624129,-0.290199457811006));
#32648=DIRECTION('',(1.,0.,0.));
#32649=DIRECTION('',(0.,-0.956966182624129,-0.290199457811006));
#32650=DIRECTION('center_axis',(1.,0.,0.));
#32651=DIRECTION('ref_axis',(0.,-0.342020143325669,-0.939692620785908));
#32652=DIRECTION('center_axis',(-1.,0.,0.));
#32653=DIRECTION('ref_axis',(0.,1.,0.));
#32654=DIRECTION('',(0.,0.546542010633327,-0.837431687132079));
#32655=DIRECTION('center_axis',(0.,-0.837431687132079,-0.546542010633327));
#32656=DIRECTION('ref_axis',(0.,0.546542010633327,-0.837431687132079));
#32657=DIRECTION('',(1.,0.,0.));
#32658=DIRECTION('',(0.,0.546542010633327,-0.837431687132079));
#32659=DIRECTION('center_axis',(1.,0.,0.));
#32660=DIRECTION('ref_axis',(0.,-0.342020143325669,-0.939692620785908));
#32661=DIRECTION('center_axis',(1.,0.,0.));
#32662=DIRECTION('ref_axis',(0.,1.,0.));
#32663=DIRECTION('center_axis',(0.,-0.11961524227066,0.992820323027551));
#32664=DIRECTION('ref_axis',(0.,-0.992820323027551,-0.11961524227066));
#32665=DIRECTION('',(-1.,0.,0.));
#32666=DIRECTION('',(0.,-0.992820323027551,-0.11961524227066));
#32667=DIRECTION('',(1.,0.,0.));
#32668=DIRECTION('',(0.,-0.992820323027551,-0.11961524227066));
#32669=DIRECTION('center_axis',(1.,0.,0.));
#32670=DIRECTION('ref_axis',(0.,-0.5,-0.866025403784438));
#32671=DIRECTION('center_axis',(-1.,0.,0.));
#32672=DIRECTION('ref_axis',(0.,1.,0.));
#32673=DIRECTION('',(0.,0.392820323027553,-0.919615242270662));
#32674=DIRECTION('center_axis',(0.,-0.919615242270662,-0.392820323027553));
#32675=DIRECTION('ref_axis',(0.,0.392820323027553,-0.919615242270662));
#32676=DIRECTION('',(1.,0.,0.));
#32677=DIRECTION('',(0.,0.392820323027553,-0.919615242270662));
#32678=DIRECTION('center_axis',(1.,0.,0.));
#32679=DIRECTION('ref_axis',(0.,-0.5,-0.866025403784438));
#32680=DIRECTION('center_axis',(1.,0.,0.));
#32681=DIRECTION('ref_axis',(0.,1.,0.));
#32682=DIRECTION('center_axis',(0.,0.0546034218778482,0.998508120307106));
#32683=DIRECTION('ref_axis',(0.,-0.998508120307106,0.0546034218778482));
#32684=DIRECTION('',(-1.,0.,0.));
#32685=DIRECTION('',(0.,-0.998508120307106,0.0546034218778482));
#32686=DIRECTION('',(1.,0.,0.));
#32687=DIRECTION('',(0.,-0.998508120307106,0.0546034218778482));
#32688=DIRECTION('center_axis',(1.,0.,0.));
#32689=DIRECTION('ref_axis',(0.,-0.64278760968654,-0.766044443118978));
#32690=DIRECTION('center_axis',(-1.,0.,0.));
#32691=DIRECTION('ref_axis',(0.,1.,0.));
#32692=DIRECTION('',(0.,0.227162988683261,-0.973856753620618));
#32693=DIRECTION('center_axis',(0.,-0.973856753620618,-0.227162988683262));
#32694=DIRECTION('ref_axis',(0.,0.227162988683261,-0.973856753620618));
#32695=DIRECTION('',(1.,0.,0.));
#32696=DIRECTION('',(0.,0.227162988683261,-0.973856753620618));
#32697=DIRECTION('center_axis',(1.,0.,0.));
#32698=DIRECTION('ref_axis',(0.,-0.64278760968654,-0.766044443118978));
#32699=DIRECTION('center_axis',(1.,0.,0.));
#32700=DIRECTION('ref_axis',(0.,1.,0.));
#32701=DIRECTION('center_axis',(0.,0.227162988683262,0.973856753620618));
#32702=DIRECTION('ref_axis',(0.,-0.973856753620618,0.227162988683262));
#32703=DIRECTION('',(-1.,0.,0.));
#32704=DIRECTION('',(0.,-0.973856753620618,0.227162988683262));
#32705=DIRECTION('',(1.,0.,0.));
#32706=DIRECTION('',(0.,-0.973856753620618,0.227162988683262));
#32707=DIRECTION('center_axis',(1.,0.,0.));
#32708=DIRECTION('ref_axis',(0.,-0.766044443118978,-0.642787609686539));
#32709=DIRECTION('center_axis',(-1.,0.,0.));
#32710=DIRECTION('ref_axis',(0.,1.,0.));
#32711=DIRECTION('',(0.,0.0546034218778476,-0.998508120307106));
#32712=DIRECTION('center_axis',(0.,-0.998508120307106,-0.0546034218778476));
#32713=DIRECTION('ref_axis',(0.,0.0546034218778476,-0.998508120307106));
#32714=DIRECTION('',(1.,0.,0.));
#32715=DIRECTION('',(0.,0.0546034218778476,-0.998508120307106));
#32716=DIRECTION('center_axis',(1.,0.,0.));
#32717=DIRECTION('ref_axis',(0.,-0.766044443118978,-0.642787609686539));
#32718=DIRECTION('center_axis',(1.,0.,0.));
#32719=DIRECTION('ref_axis',(0.,1.,0.));
#32720=DIRECTION('center_axis',(0.,0.392820323027554,0.919615242270662));
#32721=DIRECTION('ref_axis',(0.,-0.919615242270662,0.392820323027554));
#32722=DIRECTION('',(-1.,0.,0.));
#32723=DIRECTION('',(0.,-0.919615242270662,0.392820323027554));
#32724=DIRECTION('',(1.,0.,0.));
#32725=DIRECTION('',(0.,-0.919615242270662,0.392820323027554));
#32726=DIRECTION('center_axis',(1.,0.,0.));
#32727=DIRECTION('ref_axis',(0.,-0.866025403784439,-0.5));
#32728=DIRECTION('center_axis',(-1.,0.,0.));
#32729=DIRECTION('ref_axis',(0.,1.,0.));
#32730=DIRECTION('',(0.,-0.11961524227066,-0.992820323027551));
#32731=DIRECTION('center_axis',(0.,-0.992820323027551,0.11961524227066));
#32732=DIRECTION('ref_axis',(0.,-0.11961524227066,-0.992820323027551));
#32733=DIRECTION('',(1.,0.,0.));
#32734=DIRECTION('',(0.,-0.11961524227066,-0.992820323027551));
#32735=DIRECTION('center_axis',(1.,0.,0.));
#32736=DIRECTION('ref_axis',(0.,-0.866025403784439,-0.5));
#32737=DIRECTION('center_axis',(1.,0.,0.));
#32738=DIRECTION('ref_axis',(0.,1.,0.));
#32739=DIRECTION('center_axis',(0.,0.546542010633329,0.837431687132078));
#32740=DIRECTION('ref_axis',(0.,-0.837431687132078,0.546542010633329));
#32741=DIRECTION('',(-1.,0.,0.));
#32742=DIRECTION('',(0.,-0.837431687132078,0.546542010633329));
#32743=DIRECTION('',(1.,0.,0.));
#32744=DIRECTION('',(0.,-0.837431687132078,0.546542010633329));
#32745=DIRECTION('center_axis',(1.,0.,0.));
#32746=DIRECTION('ref_axis',(0.,-0.939692620785909,-0.342020143325668));
#32747=DIRECTION('center_axis',(-1.,0.,0.));
#32748=DIRECTION('ref_axis',(0.,1.,0.));
#32749=DIRECTION('',(0.,-0.290199457811008,-0.956966182624129));
#32750=DIRECTION('center_axis',(0.,-0.956966182624129,0.290199457811008));
#32751=DIRECTION('ref_axis',(0.,-0.290199457811008,-0.956966182624129));
#32752=DIRECTION('',(1.,0.,0.));
#32753=DIRECTION('',(0.,-0.290199457811008,-0.956966182624129));
#32754=DIRECTION('center_axis',(1.,0.,0.));
#32755=DIRECTION('ref_axis',(0.,-0.939692620785909,-0.342020143325668));
#32756=DIRECTION('center_axis',(1.,0.,0.));
#32757=DIRECTION('ref_axis',(0.,1.,0.));
#32758=DIRECTION('center_axis',(0.,0.683657295809611,0.729803193940867));
#32759=DIRECTION('ref_axis',(0.,-0.729803193940867,0.683657295809611));
#32760=DIRECTION('',(-1.,0.,0.));
#32761=DIRECTION('',(0.,-0.729803193940867,0.683657295809611));
#32762=DIRECTION('',(1.,0.,0.));
#32763=DIRECTION('',(0.,-0.729803193940867,0.683657295809611));
#32764=DIRECTION('center_axis',(1.,0.,0.));
#32765=DIRECTION('ref_axis',(0.,-0.984807753012208,-0.17364817766693));
#32766=DIRECTION('center_axis',(-1.,0.,0.));
#32767=DIRECTION('ref_axis',(0.,1.,0.));
#32768=DIRECTION('',(0.,-0.451966109673778,-0.892035109009926));
#32769=DIRECTION('center_axis',(0.,-0.892035109009926,0.451966109673778));
#32770=DIRECTION('ref_axis',(0.,-0.451966109673778,-0.892035109009926));
#32771=DIRECTION('',(1.,0.,0.));
#32772=DIRECTION('',(0.,-0.451966109673778,-0.892035109009926));
#32773=DIRECTION('center_axis',(1.,0.,0.));
#32774=DIRECTION('ref_axis',(0.,-0.984807753012208,-0.17364817766693));
#32775=DIRECTION('center_axis',(1.,0.,0.));
#32776=DIRECTION('ref_axis',(0.,1.,0.));
#32777=DIRECTION('center_axis',(0.,0.800000000000002,0.599999999999997));
#32778=DIRECTION('ref_axis',(0.,-0.599999999999997,0.800000000000002));
#32779=DIRECTION('',(-1.,0.,0.));
#32780=DIRECTION('',(0.,-0.599999999999997,0.800000000000002));
#32781=DIRECTION('',(1.,0.,0.));
#32782=DIRECTION('',(0.,-0.599999999999997,0.800000000000002));
#32783=DIRECTION('center_axis',(1.,0.,0.));
#32784=DIRECTION('ref_axis',(0.,-1.,1.83697019872103E-16));
#32785=DIRECTION('center_axis',(-1.,0.,0.));
#32786=DIRECTION('ref_axis',(0.,1.,0.));
#32787=DIRECTION('',(0.,-0.599999999999998,-0.800000000000002));
#32788=DIRECTION('center_axis',(0.,-0.800000000000002,0.599999999999998));
#32789=DIRECTION('ref_axis',(0.,-0.599999999999998,-0.800000000000002));
#32790=DIRECTION('',(1.,0.,0.));
#32791=DIRECTION('',(0.,-0.599999999999998,-0.800000000000002));
#32792=DIRECTION('center_axis',(1.,0.,0.));
#32793=DIRECTION('ref_axis',(0.,-1.,1.83697019872103E-16));
#32794=DIRECTION('center_axis',(1.,0.,0.));
#32795=DIRECTION('ref_axis',(0.,1.,0.));
#32796=DIRECTION('center_axis',(0.,0.892035109009926,0.451966109673778));
#32797=DIRECTION('ref_axis',(0.,-0.451966109673778,0.892035109009926));
#32798=DIRECTION('',(-1.,0.,0.));
#32799=DIRECTION('',(0.,-0.451966109673778,0.892035109009926));
#32800=DIRECTION('',(1.,0.,0.));
#32801=DIRECTION('',(0.,-0.451966109673778,0.892035109009926));
#32802=DIRECTION('center_axis',(1.,0.,0.));
#32803=DIRECTION('ref_axis',(0.,-0.984807753012208,0.17364817766693));
#32804=DIRECTION('center_axis',(-1.,0.,0.));
#32805=DIRECTION('ref_axis',(0.,1.,0.));
#32806=DIRECTION('',(0.,-0.729803193940867,-0.683657295809611));
#32807=DIRECTION('center_axis',(0.,-0.683657295809611,0.729803193940867));
#32808=DIRECTION('ref_axis',(0.,-0.729803193940867,-0.683657295809611));
#32809=DIRECTION('',(1.,0.,0.));
#32810=DIRECTION('',(0.,-0.729803193940867,-0.683657295809611));
#32811=DIRECTION('center_axis',(1.,0.,0.));
#32812=DIRECTION('ref_axis',(0.,-0.984807753012208,0.17364817766693));
#32813=DIRECTION('center_axis',(1.,0.,0.));
#32814=DIRECTION('ref_axis',(0.,1.,0.));
#32815=DIRECTION('center_axis',(0.,0.956966182624129,0.290199457811006));
#32816=DIRECTION('ref_axis',(0.,-0.290199457811006,0.956966182624129));
#32817=DIRECTION('',(-1.,0.,0.));
#32818=DIRECTION('',(0.,-0.290199457811006,0.956966182624129));
#32819=DIRECTION('',(1.,0.,0.));
#32820=DIRECTION('',(0.,-0.290199457811006,0.956966182624129));
#32821=DIRECTION('center_axis',(1.,0.,0.));
#32822=DIRECTION('ref_axis',(0.,-0.939692620785908,0.342020143325669));
#32823=DIRECTION('center_axis',(-1.,0.,0.));
#32824=DIRECTION('ref_axis',(0.,1.,0.));
#32825=DIRECTION('',(0.,-0.837431687132079,-0.546542010633328));
#32826=DIRECTION('center_axis',(0.,-0.546542010633328,0.837431687132079));
#32827=DIRECTION('ref_axis',(0.,-0.837431687132079,-0.546542010633328));
#32828=DIRECTION('',(1.,0.,0.));
#32829=DIRECTION('',(0.,-0.837431687132079,-0.546542010633328));
#32830=DIRECTION('center_axis',(1.,0.,0.));
#32831=DIRECTION('ref_axis',(0.,-0.939692620785908,0.342020143325669));
#32832=DIRECTION('center_axis',(1.,0.,0.));
#32833=DIRECTION('ref_axis',(0.,1.,0.));
#32834=DIRECTION('center_axis',(0.,0.992820323027551,0.11961524227066));
#32835=DIRECTION('ref_axis',(0.,-0.11961524227066,0.992820323027551));
#32836=DIRECTION('',(-1.,0.,0.));
#32837=DIRECTION('',(0.,-0.11961524227066,0.992820323027551));
#32838=DIRECTION('',(1.,0.,0.));
#32839=DIRECTION('',(0.,-0.11961524227066,0.992820323027551));
#32840=DIRECTION('center_axis',(1.,0.,0.));
#32841=DIRECTION('ref_axis',(0.,-0.866025403784438,0.5));
#32842=DIRECTION('center_axis',(-1.,0.,0.));
#32843=DIRECTION('ref_axis',(0.,1.,0.));
#32844=DIRECTION('',(0.,-0.919615242270662,-0.392820323027553));
#32845=DIRECTION('center_axis',(0.,-0.392820323027553,0.919615242270662));
#32846=DIRECTION('ref_axis',(0.,-0.919615242270662,-0.392820323027553));
#32847=DIRECTION('',(1.,0.,0.));
#32848=DIRECTION('',(0.,-0.919615242270662,-0.392820323027553));
#32849=DIRECTION('center_axis',(1.,0.,0.));
#32850=DIRECTION('ref_axis',(0.,-0.866025403784438,0.5));
#32851=DIRECTION('center_axis',(1.,0.,0.));
#32852=DIRECTION('ref_axis',(0.,1.,0.));
#32853=DIRECTION('center_axis',(0.,0.998508120307106,-0.054603421877848));
#32854=DIRECTION('ref_axis',(0.,0.054603421877848,0.998508120307106));
#32855=DIRECTION('',(-1.,0.,0.));
#32856=DIRECTION('',(0.,0.054603421877848,0.998508120307106));
#32857=DIRECTION('',(1.,0.,0.));
#32858=DIRECTION('',(0.,0.054603421877848,0.998508120307106));
#32859=DIRECTION('center_axis',(1.,0.,0.));
#32860=DIRECTION('ref_axis',(0.,-0.766044443118978,0.642787609686539));
#32861=DIRECTION('center_axis',(-1.,0.,0.));
#32862=DIRECTION('ref_axis',(0.,1.,0.));
#32863=DIRECTION('',(0.,-0.973856753620618,-0.227162988683262));
#32864=DIRECTION('center_axis',(0.,-0.227162988683262,0.973856753620618));
#32865=DIRECTION('ref_axis',(0.,-0.973856753620618,-0.227162988683262));
#32866=DIRECTION('',(1.,0.,0.));
#32867=DIRECTION('',(0.,-0.973856753620618,-0.227162988683262));
#32868=DIRECTION('center_axis',(1.,0.,0.));
#32869=DIRECTION('ref_axis',(0.,-0.766044443118978,0.642787609686539));
#32870=DIRECTION('center_axis',(1.,0.,0.));
#32871=DIRECTION('ref_axis',(0.,1.,0.));
#32872=DIRECTION('center_axis',(0.,0.973856753620618,-0.227162988683262));
#32873=DIRECTION('ref_axis',(0.,0.227162988683262,0.973856753620618));
#32874=DIRECTION('',(-1.,0.,0.));
#32875=DIRECTION('',(0.,0.227162988683262,0.973856753620618));
#32876=DIRECTION('',(1.,0.,0.));
#32877=DIRECTION('',(0.,0.227162988683262,0.973856753620618));
#32878=DIRECTION('center_axis',(1.,0.,0.));
#32879=DIRECTION('ref_axis',(0.,-0.642787609686539,0.766044443118978));
#32880=DIRECTION('center_axis',(-1.,0.,0.));
#32881=DIRECTION('ref_axis',(0.,1.,0.));
#32882=DIRECTION('',(0.,-0.998508120307106,-0.0546034218778477));
#32883=DIRECTION('center_axis',(0.,-0.0546034218778477,0.998508120307106));
#32884=DIRECTION('ref_axis',(0.,-0.998508120307106,-0.0546034218778477));
#32885=DIRECTION('',(1.,0.,0.));
#32886=DIRECTION('',(0.,-0.998508120307106,-0.0546034218778477));
#32887=DIRECTION('center_axis',(1.,0.,0.));
#32888=DIRECTION('ref_axis',(0.,-0.642787609686539,0.766044443118978));
#32889=DIRECTION('center_axis',(1.,0.,0.));
#32890=DIRECTION('ref_axis',(0.,1.,0.));
#32891=DIRECTION('center_axis',(0.,0.919615242270662,-0.392820323027554));
#32892=DIRECTION('ref_axis',(0.,0.392820323027554,0.919615242270662));
#32893=DIRECTION('',(-1.,0.,0.));
#32894=DIRECTION('',(0.,0.392820323027554,0.919615242270662));
#32895=DIRECTION('',(1.,0.,0.));
#32896=DIRECTION('',(0.,0.392820323027554,0.919615242270662));
#32897=DIRECTION('center_axis',(1.,0.,0.));
#32898=DIRECTION('ref_axis',(0.,-0.5,0.866025403784439));
#32899=DIRECTION('center_axis',(-1.,0.,0.));
#32900=DIRECTION('ref_axis',(0.,1.,0.));
#32901=DIRECTION('',(0.,-0.992820323027551,0.11961524227066));
#32902=DIRECTION('center_axis',(0.,0.11961524227066,0.992820323027551));
#32903=DIRECTION('ref_axis',(0.,-0.992820323027551,0.11961524227066));
#32904=DIRECTION('',(1.,0.,0.));
#32905=DIRECTION('',(0.,-0.992820323027551,0.11961524227066));
#32906=DIRECTION('center_axis',(1.,0.,0.));
#32907=DIRECTION('ref_axis',(0.,-0.5,0.866025403784439));
#32908=DIRECTION('center_axis',(1.,0.,0.));
#32909=DIRECTION('ref_axis',(0.,1.,0.));
#32910=DIRECTION('center_axis',(0.,0.837431687132078,-0.546542010633328));
#32911=DIRECTION('ref_axis',(0.,0.546542010633328,0.837431687132078));
#32912=DIRECTION('',(-1.,0.,0.));
#32913=DIRECTION('',(0.,0.546542010633328,0.837431687132078));
#32914=DIRECTION('',(1.,0.,0.));
#32915=DIRECTION('',(0.,0.546542010633328,0.837431687132078));
#32916=DIRECTION('center_axis',(1.,0.,0.));
#32917=DIRECTION('ref_axis',(0.,-0.342020143325669,0.939692620785909));
#32918=DIRECTION('center_axis',(-1.,0.,0.));
#32919=DIRECTION('ref_axis',(0.,1.,0.));
#32920=DIRECTION('',(0.,-0.956966182624129,0.290199457811007));
#32921=DIRECTION('center_axis',(0.,0.290199457811007,0.956966182624129));
#32922=DIRECTION('ref_axis',(0.,-0.956966182624129,0.290199457811007));
#32923=DIRECTION('',(1.,0.,0.));
#32924=DIRECTION('',(0.,-0.956966182624129,0.290199457811007));
#32925=DIRECTION('center_axis',(1.,0.,0.));
#32926=DIRECTION('ref_axis',(0.,-0.342020143325669,0.939692620785909));
#32927=DIRECTION('center_axis',(1.,0.,0.));
#32928=DIRECTION('ref_axis',(0.,1.,0.));
#32929=DIRECTION('center_axis',(0.,0.729803193940867,-0.683657295809611));
#32930=DIRECTION('ref_axis',(0.,0.683657295809611,0.729803193940867));
#32931=DIRECTION('',(-1.,0.,0.));
#32932=DIRECTION('',(0.,0.683657295809611,0.729803193940867));
#32933=DIRECTION('',(1.,0.,0.));
#32934=DIRECTION('',(0.,0.683657295809611,0.729803193940867));
#32935=DIRECTION('center_axis',(1.,0.,0.));
#32936=DIRECTION('ref_axis',(0.,-0.17364817766693,0.984807753012208));
#32937=DIRECTION('center_axis',(-1.,0.,0.));
#32938=DIRECTION('ref_axis',(0.,1.,0.));
#32939=DIRECTION('',(0.,-0.892035109009926,0.451966109673778));
#32940=DIRECTION('center_axis',(0.,0.451966109673778,0.892035109009926));
#32941=DIRECTION('ref_axis',(0.,-0.892035109009926,0.451966109673778));
#32942=DIRECTION('',(1.,0.,0.));
#32943=DIRECTION('',(0.,-0.892035109009926,0.451966109673778));
#32944=DIRECTION('center_axis',(1.,0.,0.));
#32945=DIRECTION('ref_axis',(0.,-0.17364817766693,0.984807753012208));
#32946=DIRECTION('center_axis',(1.,0.,0.));
#32947=DIRECTION('ref_axis',(0.,1.,0.));
#32948=DIRECTION('center_axis',(0.,0.599999999999997,-0.800000000000002));
#32949=DIRECTION('ref_axis',(0.,0.800000000000002,0.599999999999997));
#32950=DIRECTION('',(-1.,0.,0.));
#32951=DIRECTION('',(0.,0.800000000000002,0.599999999999997));
#32952=DIRECTION('',(1.,0.,0.));
#32953=DIRECTION('',(0.,0.800000000000002,0.599999999999997));
#32954=DIRECTION('center_axis',(1.,0.,0.));
#32955=DIRECTION('ref_axis',(0.,1.22464679914735E-16,1.));
#32956=DIRECTION('center_axis',(-1.,0.,0.));
#32957=DIRECTION('ref_axis',(0.,1.,0.));
#32958=DIRECTION('',(0.,-0.800000000000002,0.599999999999998));
#32959=DIRECTION('center_axis',(-1.,0.,0.));
#32960=DIRECTION('ref_axis',(0.,1.,0.));
#32961=DIRECTION('center_axis',(0.,0.599999999999998,0.800000000000002));
#32962=DIRECTION('ref_axis',(0.,-0.800000000000002,0.599999999999998));
#32963=DIRECTION('',(1.,0.,0.));
#32964=DIRECTION('',(0.,-0.800000000000002,0.599999999999998));
#32965=DIRECTION('center_axis',(1.,0.,0.));
#32966=DIRECTION('ref_axis',(0.,1.22464679914735E-16,1.));
#32967=DIRECTION('center_axis',(1.,0.,0.));
#32968=DIRECTION('ref_axis',(0.,1.,0.));
#32969=DIRECTION('center_axis',(1.,0.,0.));
#32970=DIRECTION('ref_axis',(0.,1.,0.));
#32971=DIRECTION('center_axis',(0.,0.451966109673778,-0.892035109009926));
#32972=DIRECTION('ref_axis',(0.,0.892035109009926,0.451966109673777));
#32973=DIRECTION('',(-1.,0.,0.));
#32974=DIRECTION('',(0.,0.892035109009926,0.451966109673777));
#32975=DIRECTION('',(1.,0.,0.));
#32976=DIRECTION('',(0.,0.892035109009926,0.451966109673777));
#32977=DIRECTION('center_axis',(1.,0.,0.));
#32978=DIRECTION('ref_axis',(0.,0.173648177666931,0.984807753012208));
#32979=DIRECTION('center_axis',(-1.,0.,0.));
#32980=DIRECTION('ref_axis',(0.,1.,0.));
#32981=DIRECTION('',(0.,-0.68365729580961,0.729803193940867));
#32982=DIRECTION('center_axis',(0.,0.729803193940867,0.68365729580961));
#32983=DIRECTION('ref_axis',(0.,-0.68365729580961,0.729803193940867));
#32984=DIRECTION('',(1.,0.,0.));
#32985=DIRECTION('',(0.,-0.68365729580961,0.729803193940867));
#32986=DIRECTION('center_axis',(1.,0.,0.));
#32987=DIRECTION('ref_axis',(0.,0.173648177666931,0.984807753012208));
#32988=DIRECTION('center_axis',(1.,0.,0.));
#32989=DIRECTION('ref_axis',(0.,1.,0.));
#32990=DIRECTION('center_axis',(0.,0.290199457811007,-0.956966182624129));
#32991=DIRECTION('ref_axis',(0.,0.956966182624129,0.290199457811007));
#32992=DIRECTION('',(-1.,0.,0.));
#32993=DIRECTION('',(0.,0.956966182624129,0.290199457811007));
#32994=DIRECTION('',(1.,0.,0.));
#32995=DIRECTION('',(0.,0.956966182624129,0.290199457811007));
#32996=DIRECTION('center_axis',(1.,0.,0.));
#32997=DIRECTION('ref_axis',(0.,0.342020143325669,0.939692620785908));
#32998=DIRECTION('center_axis',(-1.,0.,0.));
#32999=DIRECTION('ref_axis',(0.,1.,0.));
#33000=DIRECTION('',(0.,-0.546542010633328,0.837431687132078));
#33001=DIRECTION('center_axis',(0.,0.837431687132078,0.546542010633328));
#33002=DIRECTION('ref_axis',(0.,-0.546542010633328,0.837431687132078));
#33003=DIRECTION('',(1.,0.,0.));
#33004=DIRECTION('',(0.,-0.546542010633328,0.837431687132078));
#33005=DIRECTION('center_axis',(1.,0.,0.));
#33006=DIRECTION('ref_axis',(0.,0.342020143325669,0.939692620785908));
#33007=DIRECTION('center_axis',(1.,0.,0.));
#33008=DIRECTION('ref_axis',(0.,1.,0.));
#33009=DIRECTION('center_axis',(0.,0.11961524227066,-0.992820323027551));
#33010=DIRECTION('ref_axis',(0.,0.992820323027551,0.11961524227066));
#33011=DIRECTION('',(-1.,0.,0.));
#33012=DIRECTION('',(0.,0.992820323027551,0.11961524227066));
#33013=DIRECTION('',(1.,0.,0.));
#33014=DIRECTION('',(0.,0.992820323027551,0.11961524227066));
#33015=DIRECTION('center_axis',(1.,0.,0.));
#33016=DIRECTION('ref_axis',(0.,0.5,0.866025403784439));
#33017=DIRECTION('center_axis',(-1.,0.,0.));
#33018=DIRECTION('ref_axis',(0.,1.,0.));
#33019=DIRECTION('',(0.,-0.392820323027554,0.919615242270662));
#33020=DIRECTION('center_axis',(0.,0.919615242270662,0.392820323027554));
#33021=DIRECTION('ref_axis',(0.,-0.392820323027554,0.919615242270662));
#33022=DIRECTION('',(1.,0.,0.));
#33023=DIRECTION('',(0.,-0.392820323027554,0.919615242270662));
#33024=DIRECTION('center_axis',(1.,0.,0.));
#33025=DIRECTION('ref_axis',(0.,0.5,0.866025403784439));
#33026=DIRECTION('center_axis',(1.,0.,0.));
#33027=DIRECTION('ref_axis',(0.,1.,0.));
#33028=DIRECTION('center_axis',(0.,-0.054603421877848,-0.998508120307106));
#33029=DIRECTION('ref_axis',(0.,0.998508120307106,-0.054603421877848));
#33030=DIRECTION('',(-1.,0.,0.));
#33031=DIRECTION('',(0.,0.998508120307106,-0.054603421877848));
#33032=DIRECTION('',(1.,0.,0.));
#33033=DIRECTION('',(0.,0.998508120307106,-0.054603421877848));
#33034=DIRECTION('center_axis',(1.,0.,0.));
#33035=DIRECTION('ref_axis',(0.,0.642787609686539,0.766044443118978));
#33036=DIRECTION('center_axis',(-1.,0.,0.));
#33037=DIRECTION('ref_axis',(0.,1.,0.));
#33038=DIRECTION('',(0.,-0.227162988683262,0.973856753620618));
#33039=DIRECTION('center_axis',(0.,0.973856753620618,0.227162988683262));
#33040=DIRECTION('ref_axis',(0.,-0.227162988683262,0.973856753620618));
#33041=DIRECTION('',(1.,0.,0.));
#33042=DIRECTION('',(0.,-0.227162988683262,0.973856753620618));
#33043=DIRECTION('center_axis',(1.,0.,0.));
#33044=DIRECTION('ref_axis',(0.,0.642787609686539,0.766044443118978));
#33045=DIRECTION('center_axis',(1.,0.,0.));
#33046=DIRECTION('ref_axis',(0.,1.,0.));
#33047=DIRECTION('center_axis',(0.,-0.227162988683262,-0.973856753620618));
#33048=DIRECTION('ref_axis',(0.,0.973856753620618,-0.227162988683262));
#33049=DIRECTION('',(-1.,0.,0.));
#33050=DIRECTION('',(0.,0.973856753620618,-0.227162988683262));
#33051=DIRECTION('',(1.,0.,0.));
#33052=DIRECTION('',(0.,0.973856753620618,-0.227162988683262));
#33053=DIRECTION('center_axis',(1.,0.,0.));
#33054=DIRECTION('ref_axis',(0.,0.766044443118978,0.642787609686539));
#33055=DIRECTION('center_axis',(-1.,0.,0.));
#33056=DIRECTION('ref_axis',(0.,1.,0.));
#33057=DIRECTION('',(0.,-0.0546034218778478,0.998508120307106));
#33058=DIRECTION('center_axis',(0.,0.998508120307106,0.0546034218778478));
#33059=DIRECTION('ref_axis',(0.,-0.0546034218778478,0.998508120307106));
#33060=DIRECTION('',(1.,0.,0.));
#33061=DIRECTION('',(0.,-0.0546034218778478,0.998508120307106));
#33062=DIRECTION('center_axis',(1.,0.,0.));
#33063=DIRECTION('ref_axis',(0.,0.766044443118978,0.642787609686539));
#33064=DIRECTION('center_axis',(1.,0.,0.));
#33065=DIRECTION('ref_axis',(0.,1.,0.));
#33066=DIRECTION('center_axis',(0.,-0.392820323027554,-0.919615242270662));
#33067=DIRECTION('ref_axis',(0.,0.919615242270662,-0.392820323027554));
#33068=DIRECTION('',(-1.,0.,0.));
#33069=DIRECTION('',(0.,0.919615242270662,-0.392820323027554));
#33070=DIRECTION('',(1.,0.,0.));
#33071=DIRECTION('',(0.,0.919615242270662,-0.392820323027554));
#33072=DIRECTION('center_axis',(1.,0.,0.));
#33073=DIRECTION('ref_axis',(0.,0.866025403784439,0.5));
#33074=DIRECTION('center_axis',(-1.,0.,0.));
#33075=DIRECTION('ref_axis',(0.,1.,0.));
#33076=DIRECTION('',(0.,0.11961524227066,0.992820323027551));
#33077=DIRECTION('center_axis',(0.,0.992820323027551,-0.11961524227066));
#33078=DIRECTION('ref_axis',(0.,0.11961524227066,0.992820323027551));
#33079=DIRECTION('',(1.,0.,0.));
#33080=DIRECTION('',(0.,0.11961524227066,0.992820323027551));
#33081=DIRECTION('center_axis',(1.,0.,0.));
#33082=DIRECTION('ref_axis',(0.,0.866025403784439,0.5));
#33083=DIRECTION('center_axis',(1.,0.,0.));
#33084=DIRECTION('ref_axis',(0.,1.,0.));
#33085=DIRECTION('center_axis',(0.,-0.546542010633328,-0.837431687132078));
#33086=DIRECTION('ref_axis',(0.,0.837431687132078,-0.546542010633328));
#33087=DIRECTION('',(-1.,0.,0.));
#33088=DIRECTION('',(0.,0.837431687132078,-0.546542010633328));
#33089=DIRECTION('',(1.,0.,0.));
#33090=DIRECTION('',(0.,0.837431687132078,-0.546542010633328));
#33091=DIRECTION('center_axis',(1.,0.,0.));
#33092=DIRECTION('ref_axis',(0.,0.939692620785908,0.342020143325669));
#33093=DIRECTION('center_axis',(-1.,0.,0.));
#33094=DIRECTION('ref_axis',(0.,1.,0.));
#33095=DIRECTION('',(0.,0.290199457811007,0.956966182624129));
#33096=DIRECTION('center_axis',(0.,0.956966182624129,-0.290199457811007));
#33097=DIRECTION('ref_axis',(0.,0.290199457811007,0.956966182624129));
#33098=DIRECTION('',(1.,0.,0.));
#33099=DIRECTION('',(0.,0.290199457811007,0.956966182624129));
#33100=DIRECTION('center_axis',(1.,0.,0.));
#33101=DIRECTION('ref_axis',(0.,0.939692620785908,0.342020143325669));
#33102=DIRECTION('center_axis',(1.,0.,0.));
#33103=DIRECTION('ref_axis',(0.,1.,0.));
#33104=DIRECTION('center_axis',(0.,-0.683657295809611,-0.729803193940867));
#33105=DIRECTION('ref_axis',(0.,0.729803193940867,-0.683657295809611));
#33106=DIRECTION('',(-1.,0.,0.));
#33107=DIRECTION('',(0.,0.729803193940867,-0.683657295809611));
#33108=DIRECTION('',(1.,0.,0.));
#33109=DIRECTION('',(0.,0.729803193940867,-0.683657295809611));
#33110=DIRECTION('center_axis',(1.,0.,0.));
#33111=DIRECTION('ref_axis',(0.,0.984807753012208,0.17364817766693));
#33112=DIRECTION('center_axis',(-1.,0.,0.));
#33113=DIRECTION('ref_axis',(0.,1.,0.));
#33114=DIRECTION('',(0.,0.451966109673778,0.892035109009926));
#33115=DIRECTION('center_axis',(0.,0.892035109009926,-0.451966109673778));
#33116=DIRECTION('ref_axis',(0.,0.451966109673778,0.892035109009926));
#33117=DIRECTION('',(1.,0.,0.));
#33118=DIRECTION('',(0.,0.451966109673778,0.892035109009926));
#33119=DIRECTION('center_axis',(1.,0.,0.));
#33120=DIRECTION('ref_axis',(0.,0.984807753012208,0.17364817766693));
#33121=DIRECTION('center_axis',(1.,0.,0.));
#33122=DIRECTION('ref_axis',(0.,1.,0.));
#33123=DIRECTION('center_axis',(0.,-0.800000000000002,-0.599999999999998));
#33124=DIRECTION('ref_axis',(0.,0.599999999999998,-0.800000000000002));
#33125=DIRECTION('',(-1.,0.,0.));
#33126=DIRECTION('',(0.,0.599999999999998,-0.800000000000002));
#33127=DIRECTION('',(1.,0.,0.));
#33128=DIRECTION('',(0.,0.599999999999998,-0.800000000000002));
#33129=DIRECTION('center_axis',(1.,0.,0.));
#33130=DIRECTION('ref_axis',(0.,1.,-6.12323399573677E-17));
#33131=DIRECTION('center_axis',(-1.,0.,0.));
#33132=DIRECTION('ref_axis',(0.,1.,0.));
#33133=DIRECTION('',(0.,0.599999999999998,0.800000000000002));
#33134=DIRECTION('center_axis',(0.,0.800000000000002,-0.599999999999998));
#33135=DIRECTION('ref_axis',(0.,0.599999999999998,0.800000000000002));
#33136=DIRECTION('',(1.,0.,0.));
#33137=DIRECTION('',(0.,0.599999999999998,0.800000000000002));
#33138=DIRECTION('center_axis',(1.,0.,0.));
#33139=DIRECTION('ref_axis',(0.,1.,-6.12323399573677E-17));
#33140=DIRECTION('center_axis',(1.,0.,0.));
#33141=DIRECTION('ref_axis',(0.,1.,0.));
#33142=DIRECTION('center_axis',(0.,-0.892035109009926,-0.451966109673778));
#33143=DIRECTION('ref_axis',(0.,0.451966109673778,-0.892035109009926));
#33144=DIRECTION('',(-1.,0.,0.));
#33145=DIRECTION('',(0.,0.451966109673778,-0.892035109009926));
#33146=DIRECTION('',(1.,0.,0.));
#33147=DIRECTION('',(0.,0.451966109673778,-0.892035109009926));
#33148=DIRECTION('center_axis',(1.,0.,0.));
#33149=DIRECTION('ref_axis',(0.,0.984807753012208,-0.17364817766693));
#33150=DIRECTION('center_axis',(-1.,0.,0.));
#33151=DIRECTION('ref_axis',(0.,1.,0.));
#33152=DIRECTION('',(0.,0.729803193940867,0.68365729580961));
#33153=DIRECTION('center_axis',(0.,0.683657295809611,-0.729803193940867));
#33154=DIRECTION('ref_axis',(0.,0.729803193940867,0.68365729580961));
#33155=DIRECTION('',(1.,0.,0.));
#33156=DIRECTION('',(0.,0.729803193940867,0.68365729580961));
#33157=DIRECTION('center_axis',(1.,0.,0.));
#33158=DIRECTION('ref_axis',(0.,0.984807753012208,-0.17364817766693));
#33159=DIRECTION('center_axis',(1.,0.,0.));
#33160=DIRECTION('ref_axis',(0.,1.,0.));
#33161=DIRECTION('center_axis',(0.,-0.956966182624129,-0.290199457811007));
#33162=DIRECTION('ref_axis',(0.,0.290199457811007,-0.956966182624129));
#33163=DIRECTION('',(-1.,0.,0.));
#33164=DIRECTION('',(0.,0.290199457811007,-0.956966182624129));
#33165=DIRECTION('',(1.,0.,0.));
#33166=DIRECTION('',(0.,0.290199457811007,-0.956966182624129));
#33167=DIRECTION('center_axis',(1.,0.,0.));
#33168=DIRECTION('ref_axis',(0.,0.939692620785908,-0.342020143325669));
#33169=DIRECTION('center_axis',(-1.,0.,0.));
#33170=DIRECTION('ref_axis',(0.,1.,0.));
#33171=DIRECTION('',(0.,0.837431687132078,0.546542010633328));
#33172=DIRECTION('center_axis',(0.,0.546542010633328,-0.837431687132078));
#33173=DIRECTION('ref_axis',(0.,0.837431687132078,0.546542010633328));
#33174=DIRECTION('',(1.,0.,0.));
#33175=DIRECTION('',(0.,0.837431687132078,0.546542010633328));
#33176=DIRECTION('center_axis',(1.,0.,0.));
#33177=DIRECTION('ref_axis',(0.,0.939692620785908,-0.342020143325669));
#33178=DIRECTION('center_axis',(1.,0.,0.));
#33179=DIRECTION('ref_axis',(0.,1.,0.));
#33180=DIRECTION('center_axis',(0.,-0.992820323027551,-0.11961524227066));
#33181=DIRECTION('ref_axis',(0.,0.11961524227066,-0.992820323027551));
#33182=DIRECTION('',(-1.,0.,0.));
#33183=DIRECTION('',(0.,0.11961524227066,-0.992820323027551));
#33184=DIRECTION('',(1.,0.,0.));
#33185=DIRECTION('',(0.,0.11961524227066,-0.992820323027551));
#33186=DIRECTION('center_axis',(1.,0.,0.));
#33187=DIRECTION('ref_axis',(0.,0.866025403784439,-0.5));
#33188=DIRECTION('center_axis',(-1.,0.,0.));
#33189=DIRECTION('ref_axis',(0.,1.,0.));
#33190=DIRECTION('',(0.,0.919615242270662,0.392820323027554));
#33191=DIRECTION('center_axis',(0.,0.392820323027554,-0.919615242270662));
#33192=DIRECTION('ref_axis',(0.,0.919615242270662,0.392820323027554));
#33193=DIRECTION('',(1.,0.,0.));
#33194=DIRECTION('',(0.,0.919615242270662,0.392820323027554));
#33195=DIRECTION('center_axis',(1.,0.,0.));
#33196=DIRECTION('ref_axis',(0.,0.866025403784439,-0.5));
#33197=DIRECTION('center_axis',(1.,0.,0.));
#33198=DIRECTION('ref_axis',(0.,1.,0.));
#33199=DIRECTION('center_axis',(0.,-0.998508120307106,0.0546034218778478));
#33200=DIRECTION('ref_axis',(0.,-0.0546034218778478,-0.998508120307106));
#33201=DIRECTION('',(-1.,0.,0.));
#33202=DIRECTION('',(0.,-0.0546034218778478,-0.998508120307106));
#33203=DIRECTION('',(1.,0.,0.));
#33204=DIRECTION('',(0.,-0.0546034218778478,-0.998508120307106));
#33205=DIRECTION('center_axis',(1.,0.,0.));
#33206=DIRECTION('ref_axis',(0.,0.766044443118978,-0.642787609686539));
#33207=DIRECTION('center_axis',(-1.,0.,0.));
#33208=DIRECTION('ref_axis',(0.,1.,0.));
#33209=DIRECTION('',(0.,0.973856753620618,0.227162988683262));
#33210=DIRECTION('center_axis',(0.,0.227162988683262,-0.973856753620618));
#33211=DIRECTION('ref_axis',(0.,0.973856753620618,0.227162988683262));
#33212=DIRECTION('',(1.,0.,0.));
#33213=DIRECTION('',(0.,0.973856753620618,0.227162988683262));
#33214=DIRECTION('center_axis',(1.,0.,0.));
#33215=DIRECTION('ref_axis',(0.,0.766044443118978,-0.642787609686539));
#33216=DIRECTION('center_axis',(1.,0.,0.));
#33217=DIRECTION('ref_axis',(0.,1.,0.));
#33218=DIRECTION('center_axis',(0.,-0.973856753620618,0.227162988683262));
#33219=DIRECTION('ref_axis',(0.,-0.227162988683262,-0.973856753620618));
#33220=DIRECTION('',(-1.,0.,0.));
#33221=DIRECTION('',(0.,-0.227162988683262,-0.973856753620618));
#33222=DIRECTION('',(1.,0.,0.));
#33223=DIRECTION('',(0.,-0.227162988683262,-0.973856753620618));
#33224=DIRECTION('center_axis',(1.,0.,0.));
#33225=DIRECTION('ref_axis',(0.,0.642787609686539,-0.766044443118978));
#33226=DIRECTION('center_axis',(-1.,0.,0.));
#33227=DIRECTION('ref_axis',(0.,1.,0.));
#33228=DIRECTION('',(0.,0.998508120307106,0.0546034218778477));
#33229=DIRECTION('center_axis',(0.,0.0546034218778477,-0.998508120307106));
#33230=DIRECTION('ref_axis',(0.,0.998508120307106,0.0546034218778477));
#33231=DIRECTION('',(1.,0.,0.));
#33232=DIRECTION('',(0.,0.998508120307106,0.0546034218778477));
#33233=DIRECTION('center_axis',(1.,0.,0.));
#33234=DIRECTION('ref_axis',(0.,0.642787609686539,-0.766044443118978));
#33235=DIRECTION('center_axis',(1.,0.,0.));
#33236=DIRECTION('ref_axis',(0.,1.,0.));
#33237=DIRECTION('center_axis',(0.,-0.919615242270662,0.392820323027554));
#33238=DIRECTION('ref_axis',(0.,-0.392820323027554,-0.919615242270662));
#33239=DIRECTION('',(-1.,0.,0.));
#33240=DIRECTION('',(0.,-0.392820323027554,-0.919615242270662));
#33241=DIRECTION('',(1.,0.,0.));
#33242=DIRECTION('',(0.,-0.392820323027554,-0.919615242270662));
#33243=DIRECTION('center_axis',(1.,0.,0.));
#33244=DIRECTION('ref_axis',(0.,0.5,-0.866025403784439));
#33245=DIRECTION('center_axis',(-1.,0.,0.));
#33246=DIRECTION('ref_axis',(0.,1.,0.));
#33247=DIRECTION('',(0.,0.992820323027551,-0.11961524227066));
#33248=DIRECTION('center_axis',(0.,-0.11961524227066,-0.992820323027551));
#33249=DIRECTION('ref_axis',(0.,0.992820323027551,-0.11961524227066));
#33250=DIRECTION('',(1.,0.,0.));
#33251=DIRECTION('',(0.,0.992820323027551,-0.11961524227066));
#33252=DIRECTION('center_axis',(1.,0.,0.));
#33253=DIRECTION('ref_axis',(0.,0.5,-0.866025403784439));
#33254=DIRECTION('center_axis',(1.,0.,0.));
#33255=DIRECTION('ref_axis',(0.,1.,0.));
#33256=DIRECTION('center_axis',(0.,-0.837431687132078,0.546542010633328));
#33257=DIRECTION('ref_axis',(0.,-0.546542010633328,-0.837431687132078));
#33258=DIRECTION('',(-1.,0.,0.));
#33259=DIRECTION('',(0.,-0.546542010633328,-0.837431687132078));
#33260=DIRECTION('',(1.,0.,0.));
#33261=DIRECTION('',(0.,-0.546542010633328,-0.837431687132078));
#33262=DIRECTION('center_axis',(1.,0.,0.));
#33263=DIRECTION('ref_axis',(0.,0.342020143325669,-0.939692620785908));
#33264=DIRECTION('center_axis',(-1.,0.,0.));
#33265=DIRECTION('ref_axis',(0.,1.,0.));
#33266=DIRECTION('',(0.,0.956966182624129,-0.290199457811007));
#33267=DIRECTION('center_axis',(0.,-0.290199457811007,-0.956966182624129));
#33268=DIRECTION('ref_axis',(0.,0.956966182624129,-0.290199457811007));
#33269=DIRECTION('',(1.,0.,0.));
#33270=DIRECTION('',(0.,0.956966182624129,-0.290199457811007));
#33271=DIRECTION('center_axis',(1.,0.,0.));
#33272=DIRECTION('ref_axis',(0.,0.342020143325669,-0.939692620785908));
#33273=DIRECTION('center_axis',(1.,0.,0.));
#33274=DIRECTION('ref_axis',(0.,1.,0.));
#33275=DIRECTION('center_axis',(0.,-0.729803193940867,0.683657295809611));
#33276=DIRECTION('ref_axis',(0.,-0.683657295809611,-0.729803193940867));
#33277=DIRECTION('',(-1.,0.,0.));
#33278=DIRECTION('',(0.,-0.683657295809611,-0.729803193940867));
#33279=DIRECTION('',(1.,0.,0.));
#33280=DIRECTION('',(0.,-0.683657295809611,-0.729803193940867));
#33281=DIRECTION('center_axis',(1.,0.,0.));
#33282=DIRECTION('ref_axis',(0.,0.17364817766693,-0.984807753012208));
#33283=DIRECTION('center_axis',(-1.,0.,0.));
#33284=DIRECTION('ref_axis',(0.,1.,0.));
#33285=DIRECTION('',(0.,0.892035109009926,-0.451966109673778));
#33286=DIRECTION('center_axis',(0.,-0.451966109673778,-0.892035109009926));
#33287=DIRECTION('ref_axis',(0.,0.892035109009926,-0.451966109673778));
#33288=DIRECTION('',(1.,0.,0.));
#33289=DIRECTION('',(0.,0.892035109009926,-0.451966109673778));
#33290=DIRECTION('center_axis',(1.,0.,0.));
#33291=DIRECTION('ref_axis',(0.,0.17364817766693,-0.984807753012208));
#33292=DIRECTION('center_axis',(1.,0.,0.));
#33293=DIRECTION('ref_axis',(0.,1.,0.));
#33294=DIRECTION('center_axis',(0.,-0.599999999999998,0.800000000000002));
#33295=DIRECTION('ref_axis',(0.,-0.800000000000002,-0.599999999999998));
#33296=DIRECTION('',(-1.,0.,0.));
#33297=DIRECTION('',(0.,-0.800000000000002,-0.599999999999998));
#33298=DIRECTION('',(1.,0.,0.));
#33299=DIRECTION('',(0.,-0.800000000000002,-0.599999999999998));
#33300=DIRECTION('center_axis',(1.,0.,0.));
#33301=DIRECTION('ref_axis',(0.,0.,-1.));
#33302=DIRECTION('center_axis',(-1.,0.,0.));
#33303=DIRECTION('ref_axis',(0.,1.,0.));
#33304=DIRECTION('',(0.,0.800000000000002,-0.599999999999998));
#33305=DIRECTION('center_axis',(0.,-0.599999999999998,-0.800000000000002));
#33306=DIRECTION('ref_axis',(0.,0.800000000000002,-0.599999999999998));
#33307=DIRECTION('',(1.,0.,0.));
#33308=DIRECTION('',(0.,0.800000000000002,-0.599999999999998));
#33309=DIRECTION('center_axis',(1.,0.,0.));
#33310=DIRECTION('ref_axis',(0.,0.,-1.));
#33311=DIRECTION('center_axis',(1.,0.,0.));
#33312=DIRECTION('ref_axis',(0.,1.,0.));
#33313=DIRECTION('center_axis',(0.,0.5,0.866025403784439));
#33314=DIRECTION('ref_axis',(0.,0.866025403784439,-0.5));
#33315=DIRECTION('',(0.,0.866025403784439,-0.5));
#33316=DIRECTION('',(-1.,0.,0.));
#33317=DIRECTION('',(0.,0.866025403784439,-0.5));
#33318=DIRECTION('',(-1.,0.,0.));
#33319=DIRECTION('center_axis',(0.,-0.5,0.866025403784439));
#33320=DIRECTION('ref_axis',(0.,0.866025403784439,0.5));
#33321=DIRECTION('',(0.,0.866025403784439,0.5));
#33322=DIRECTION('',(-1.,0.,0.));
#33323=DIRECTION('',(0.,0.866025403784439,0.5));
#33324=DIRECTION('center_axis',(0.,-1.,-1.20185167898973E-16));
#33325=DIRECTION('ref_axis',(0.,-1.20185167898973E-16,1.));
#33326=DIRECTION('',(0.,-1.20185167898973E-16,1.));
#33327=DIRECTION('',(-1.,0.,0.));
#33328=DIRECTION('',(0.,-1.20185167898973E-16,1.));
#33329=DIRECTION('center_axis',(0.,-0.5,-0.866025403784439));
#33330=DIRECTION('ref_axis',(0.,-0.866025403784439,0.5));
#33331=DIRECTION('',(0.,-0.866025403784439,0.5));
#33332=DIRECTION('',(-1.,0.,0.));
#33333=DIRECTION('',(0.,-0.866025403784439,0.5));
#33334=DIRECTION('center_axis',(0.,0.5,-0.866025403784439));
#33335=DIRECTION('ref_axis',(0.,-0.866025403784439,-0.5));
#33336=DIRECTION('',(0.,-0.866025403784439,-0.5));
#33337=DIRECTION('',(-1.,0.,0.));
#33338=DIRECTION('',(0.,-0.866025403784439,-0.5));
#33339=DIRECTION('center_axis',(0.,1.,-3.60555503696918E-16));
#33340=DIRECTION('ref_axis',(0.,-3.60555503696918E-16,-1.));
#33341=DIRECTION('',(0.,-3.60555503696918E-16,-1.));
#33342=DIRECTION('',(0.,-3.60555503696918E-16,-1.));
#33343=DIRECTION('center_axis',(-1.,0.,0.));
#33344=DIRECTION('ref_axis',(0.,0.,1.));
#33345=DIRECTION('center_axis',(-1.,0.,0.));
#33346=DIRECTION('ref_axis',(0.,0.,1.));
#33347=DIRECTION('center_axis',(1.,0.,0.));
#33348=DIRECTION('ref_axis',(0.,0.,-1.));
#33349=DIRECTION('center_axis',(1.,0.,0.));
#33350=DIRECTION('ref_axis',(0.,1.,0.));
#33351=DIRECTION('',(-0.707106781186553,0.707106781186542,8.65956056235487E-17));
#33352=DIRECTION('center_axis',(1.,0.,0.));
#33353=DIRECTION('ref_axis',(0.,-0.992415828451704,-0.122926089332239));
#33354=DIRECTION('center_axis',(-1.,0.,0.));
#33355=DIRECTION('ref_axis',(0.,1.,0.));
#33356=DIRECTION('center_axis',(-1.,0.,0.));
#33357=DIRECTION('ref_axis',(0.,1.,0.));
#33358=DIRECTION('center_axis',(1.,0.,0.));
#33359=DIRECTION('ref_axis',(0.,0.,-1.));
#33360=DIRECTION('',(0.995037190209989,0.0995037190209994,1.21856911002324E-17));
#33361=DIRECTION('center_axis',(1.,0.,0.));
#33362=DIRECTION('ref_axis',(0.,1.,0.));
#33363=DIRECTION('center_axis',(1.,0.,0.));
#33364=DIRECTION('ref_axis',(0.,0.,-1.));
#33365=DIRECTION('',(-1.,0.,0.));
#33366=DIRECTION('center_axis',(-1.,0.,0.));
#33367=DIRECTION('ref_axis',(0.,0.,1.));
#33368=DIRECTION('center_axis',(1.,0.,0.));
#33369=DIRECTION('ref_axis',(0.,0.,-1.));
#33370=DIRECTION('center_axis',(1.,0.,0.));
#33371=DIRECTION('ref_axis',(0.,1.,0.));
#33372=DIRECTION('center_axis',(1.,0.,0.));
#33373=DIRECTION('ref_axis',(0.,0.,-1.));
#33374=DIRECTION('',(-1.,0.,0.));
#33375=DIRECTION('',(-1.,0.,0.));
#33376=DIRECTION('center_axis',(-1.,0.,0.));
#33377=DIRECTION('ref_axis',(0.,1.,0.));
#33378=DIRECTION('center_axis',(1.,0.,0.));
#33379=DIRECTION('ref_axis',(0.,0.,-1.));
#33380=DIRECTION('',(-0.707106781186547,-0.707106781186548,-8.65956056235494E-17));
#33381=DIRECTION('center_axis',(1.,0.,0.));
#33382=DIRECTION('ref_axis',(0.,0.,-1.));
#33383=DIRECTION('axis',(0.,0.,1.));
#33384=DIRECTION('refdir',(1.,0.,0.));
#33385=DIRECTION('center_axis',(-1.,0.,0.));
#33386=DIRECTION('ref_axis',(0.,0.,1.));
#33387=DIRECTION('center_axis',(1.,0.,0.));
#33388=DIRECTION('ref_axis',(0.,0.,-1.));
#33389=DIRECTION('center_axis',(1.,0.,0.));
#33390=DIRECTION('ref_axis',(0.,1.,0.));
#33391=DIRECTION('center_axis',(1.,0.,0.));
#33392=DIRECTION('ref_axis',(0.,0.,-1.));
#33393=DIRECTION('',(-0.707106781186547,0.707106781186548,8.65956056235494E-17));
#33394=DIRECTION('center_axis',(1.,0.,0.));
#33395=DIRECTION('ref_axis',(0.,1.,0.));
#33396=DIRECTION('center_axis',(1.,0.,0.));
#33397=DIRECTION('ref_axis',(0.,0.,-1.));
#33398=DIRECTION('',(-1.,0.,0.));
#33399=DIRECTION('center_axis',(-1.,0.,0.));
#33400=DIRECTION('ref_axis',(0.,1.,0.));
#33401=DIRECTION('center_axis',(1.,0.,0.));
#33402=DIRECTION('ref_axis',(0.,0.,-1.));
#33403=DIRECTION('',(-0.707106781186547,-0.707106781186547,-8.65956056235493E-17));
#33404=DIRECTION('center_axis',(1.,0.,0.));
#33405=DIRECTION('ref_axis',(0.,0.,-1.));
#33406=DIRECTION('',(0.,0.,1.));
#33407=DIRECTION('',(1.,0.,0.));
#33408=DIRECTION('',(0.,0.,1.));
#33409=DIRECTION('',(1.,0.,0.));
#33410=DIRECTION('',(0.,0.,1.));
#33411=DIRECTION('',(1.,0.,0.));
#33412=DIRECTION('',(0.,0.,1.));
#33413=DIRECTION('',(1.,0.,0.));
#33414=DIRECTION('',(0.,0.,1.));
#33415=DIRECTION('',(1.,0.,0.));
#33416=DIRECTION('',(0.,0.,1.));
#33417=DIRECTION('',(1.,0.,0.));
#33418=DIRECTION('',(0.,0.,1.));
#33419=DIRECTION('',(-1.,0.,0.));
#33420=DIRECTION('',(0.,0.,-1.));
#33421=DIRECTION('',(0.,1.,0.));
#33422=DIRECTION('',(0.,0.,-1.));
#33423=DIRECTION('',(0.,1.,0.));
#33424=DIRECTION('',(0.,0.,1.));
#33425=DIRECTION('',(1.,0.,0.));
#33426=DIRECTION('',(0.,0.,1.));
#33427=DIRECTION('',(1.,0.,0.));
#33428=DIRECTION('',(0.,0.,1.));
#33429=DIRECTION('',(-1.,0.,0.));
#33430=DIRECTION('',(0.,0.,-1.));
#33431=DIRECTION('',(0.,1.,0.));
#33432=DIRECTION('',(0.,0.,-1.));
#33433=DIRECTION('',(0.,1.,0.));
#33434=DIRECTION('',(0.,0.,-1.));
#33435=DIRECTION('',(0.,1.,0.));
#33436=DIRECTION('',(0.,0.,-1.));
#33437=DIRECTION('',(0.,1.,0.));
#33438=DIRECTION('',(0.,0.,-1.));
#33439=DIRECTION('',(0.,1.,0.));
#33440=DIRECTION('',(0.,0.,-1.));
#33441=DIRECTION('',(0.,1.,0.));
#33442=DIRECTION('',(0.,0.,-1.));
#33443=DIRECTION('',(0.,1.,0.));
#33444=DIRECTION('',(0.,0.,-1.));
#33445=DIRECTION('',(0.,1.,0.));
#33446=DIRECTION('',(0.,0.,-1.));
#33447=DIRECTION('',(0.,1.,0.));
#33448=DIRECTION('',(0.,0.,-1.));
#33449=DIRECTION('',(0.,1.,0.));
#33450=DIRECTION('',(0.,0.,-1.));
#33451=DIRECTION('',(0.,1.,0.));
#33452=DIRECTION('',(0.,0.,-1.));
#33453=DIRECTION('',(0.,1.,0.));
#33454=DIRECTION('',(0.,0.,-1.));
#33455=DIRECTION('',(0.,1.,0.));
#33456=CARTESIAN_POINT('',(0.,0.,0.));
#33457=CARTESIAN_POINT('',(0.,0.,0.));
#33458=CARTESIAN_POINT('Origin',(30.5,0.25,-55.));
#33459=CARTESIAN_POINT('',(22.,0.,-55.));
#33460=CARTESIAN_POINT('Origin',(30.5,0.,-55.));
#33461=CARTESIAN_POINT('',(21.5,0.5,-55.));
#33462=CARTESIAN_POINT('',(21.75,0.25,-55.));
#33463=CARTESIAN_POINT('Origin',(30.5,0.5,-55.));
#33464=CARTESIAN_POINT('Origin',(30.5,0.,-55.));
#33465=CARTESIAN_POINT('',(24.95,0.,-55.));
#33466=CARTESIAN_POINT('Origin',(30.5,0.,-55.));
#33467=CARTESIAN_POINT('Origin',(30.5,4.,-55.));
#33468=CARTESIAN_POINT('',(21.5,4.,-55.));
#33469=CARTESIAN_POINT('',(21.5,4.,-55.));
#33470=CARTESIAN_POINT('Origin',(30.5,4.,-55.));
#33471=CARTESIAN_POINT('Origin',(-30.5,0.25,-55.));
#33472=CARTESIAN_POINT('',(-39.,0.,-55.));
#33473=CARTESIAN_POINT('Origin',(-30.5,0.,-55.));
#33474=CARTESIAN_POINT('',(-39.5,0.5,-55.));
#33475=CARTESIAN_POINT('',(-39.25,0.25,-55.));
#33476=CARTESIAN_POINT('Origin',(-30.5,0.5,-55.));
#33477=CARTESIAN_POINT('Origin',(-30.5,0.,-55.));
#33478=CARTESIAN_POINT('',(-36.05,0.,-55.));
#33479=CARTESIAN_POINT('Origin',(-30.5,0.,-55.));
#33480=CARTESIAN_POINT('Origin',(-30.5,4.,-55.));
#33481=CARTESIAN_POINT('',(-39.5,4.,-55.));
#33482=CARTESIAN_POINT('',(-39.5,4.,-55.));
#33483=CARTESIAN_POINT('Origin',(-30.5,4.,-55.));
#33484=CARTESIAN_POINT('Origin',(0.,2.35,0.));
#33485=CARTESIAN_POINT('',(-1.28587913910472E-15,2.1,10.5));
#33486=CARTESIAN_POINT('Origin',(0.,2.1,0.));
#33487=CARTESIAN_POINT('',(1.22464679914735E-15,2.6,10.));
#33488=CARTESIAN_POINT('',(-1.25526296912604E-15,2.35,10.25));
#33489=CARTESIAN_POINT('',(-1.22464679914735E-15,2.6,-10.));
#33490=CARTESIAN_POINT('Origin',(0.,2.6,0.));
#33491=CARTESIAN_POINT('Origin',(0.,2.6,0.));
#33492=CARTESIAN_POINT('Origin',(0.,10.1,0.));
#33493=CARTESIAN_POINT('',(1.22464679914735E-15,17.5,-10.));
#33494=CARTESIAN_POINT('',(-1.22464679914735E-15,10.1,-10.));
#33495=CARTESIAN_POINT('Origin',(0.,17.5,0.));
#33496=CARTESIAN_POINT('Origin',(0.,2.1,10.));
#33497=CARTESIAN_POINT('',(-1.75124492278072E-15,2.1,-14.3));
#33498=CARTESIAN_POINT('Origin',(0.,2.1,0.));
#33499=CARTESIAN_POINT('Origin',(0.,17.75,0.));
#33500=CARTESIAN_POINT('',(-1.28587913910472E-15,18.,-10.5));
#33501=CARTESIAN_POINT('Origin',(0.,18.,0.));
#33502=CARTESIAN_POINT('',(-1.25526296912604E-15,17.75,-10.25));
#33503=CARTESIAN_POINT('Origin',(0.,18.,-16.5));
#33504=CARTESIAN_POINT('',(-20.95,18.,0.));
#33505=CARTESIAN_POINT('',(-20.95,18.,-33.));
#33506=CARTESIAN_POINT('',(-20.95,18.,-24.75));
#33507=CARTESIAN_POINT('',(20.95,18.,2.5656350442137E-15));
#33508=CARTESIAN_POINT('Origin',(0.,18.,0.));
#33509=CARTESIAN_POINT('',(20.95,18.,-33.));
#33510=CARTESIAN_POINT('',(20.95,18.,-8.25));
#33511=CARTESIAN_POINT('Origin',(0.,18.,-33.));
#33512=CARTESIAN_POINT('Ctrl Pts',(-1.57453458878625,0.00185294611160958,
-63.8682453580158));
#33513=CARTESIAN_POINT('Ctrl Pts',(-1.57038661518133,0.00164657951619636,
-63.8641633585059));
#33514=CARTESIAN_POINT('Ctrl Pts',(-1.539887259118,0.000219540540016254,
-63.8342603933394));
#33515=CARTESIAN_POINT('Ctrl Pts',(-1.50642463475971,1.28888202266086E-5,
-63.8016081711826));
#33516=CARTESIAN_POINT('Ctrl Pts',(-1.50104102377551,-5.7788428237887E-19,
-63.7963365978802));
#33517=CARTESIAN_POINT('Ctrl Pts',(-1.5,0.,-63.7953186364093));
#33518=CARTESIAN_POINT('Ctrl Pts',(-1.3391048451961,0.00185294611160958,
-64.1036751016059));
#33519=CARTESIAN_POINT('Ctrl Pts',(-1.3349788629562,0.00164657951619632,
-64.0995711107311));
#33520=CARTESIAN_POINT('Ctrl Pts',(-1.30471094646532,0.000219540540016221,
-64.0694367059921));
#33521=CARTESIAN_POINT('Ctrl Pts',(-1.27147622898836,1.2888820226605E-5,
-64.0365565769539));
#33522=CARTESIAN_POINT('Ctrl Pts',(-1.26613954847708,-3.55392112035979E-19,
-64.0312380731786));
#33523=CARTESIAN_POINT('Ctrl Pts',(-1.26510621213642,0.,-64.0302124242728));
#33524=CARTESIAN_POINT('Ctrl Pts',(-1.10367510160594,0.00185294611160958,
-64.3391048451961));
#33525=CARTESIAN_POINT('Ctrl Pts',(-1.09957111073107,0.00164657951619628,
-64.3349788629562));
#33526=CARTESIAN_POINT('Ctrl Pts',(-1.0694367059921,-2.15946827128807E-5,
-64.3045339520233));
#33527=CARTESIAN_POINT('Ctrl Pts',(-1.0365565769539,0.000165305522380892,
-64.2714516442099));
#33528=CARTESIAN_POINT('Ctrl Pts',(-1.03123807317865,-1.23401226123361E-19,
-64.2661395484771));
#33529=CARTESIAN_POINT('Ctrl Pts',(-1.03021242427284,0.,-64.2651062121364));
#33530=CARTESIAN_POINT('Ctrl Pts',(-0.868245358015784,0.00185294611160958,
-64.5745345887862));
#33531=CARTESIAN_POINT('Ctrl Pts',(-0.864163358505944,0.00164657951619624,
-64.5703866151813));
#33532=CARTESIAN_POINT('Ctrl Pts',(-0.834260393339416,0.000219540540015427,
-64.539887259118));
#33533=CARTESIAN_POINT('Ctrl Pts',(-0.801608171182549,1.28888202263444E-5,
-64.5064246347597));
#33534=CARTESIAN_POINT('Ctrl Pts',(-0.796336597880214,9.63140470631229E-20,
-64.5010410237755));
#33535=CARTESIAN_POINT('Ctrl Pts',(-0.79531863640926,0.,-64.5));
#33536=CARTESIAN_POINT('',(-1.5,0.,-63.7953186364093));
#33537=CARTESIAN_POINT('',(-1.57453458878625,0.00185294611160958,-63.8682453580158));
#33538=CARTESIAN_POINT('Ctrl Pts',(-1.49999999999999,-2.22044604925031E-16,
-63.7953186364093));
#33539=CARTESIAN_POINT('Ctrl Pts',(-1.50033136103367,-2.2224081007119E-16,
-63.7956426566413));
#33540=CARTESIAN_POINT('Ctrl Pts',(-1.50066599103948,9.12216844759869E-8,
-63.7959698710105));
#33541=CARTESIAN_POINT('Ctrl Pts',(-1.50107815475909,3.87472611551587E-7,
-63.7963728195339));
#33542=CARTESIAN_POINT('Ctrl Pts',(-1.50151072778695,6.98393137628669E-7,
-63.7967957210522));
#33543=CARTESIAN_POINT('Ctrl Pts',(-1.5020284953742,1.23194503946057E-6,
-63.7973018394014));
#33544=CARTESIAN_POINT('Ctrl Pts',(-1.50267576544792,2.38657547568799E-6,
-63.7979344421873));
#33545=CARTESIAN_POINT('Ctrl Pts',(-1.50336536547683,3.6167160530659E-6,
-63.798608415722));
#33546=CARTESIAN_POINT('Ctrl Pts',(-1.50420167541466,5.55516755071447E-6,
-63.7994256794685));
#33547=CARTESIAN_POINT('Ctrl Pts',(-1.50519595537272,8.99934440767858E-6,
-63.8003972134394));
#33548=CARTESIAN_POINT('Ctrl Pts',(-1.50629355744866,1.28014281542221E-5,
-63.8014697058442));
#33549=CARTESIAN_POINT('Ctrl Pts',(-1.50758325228905,1.84658046861493E-5,
-63.802729790879));
#33550=CARTESIAN_POINT('Ctrl Pts',(-1.50903534240277,2.72127176224046E-5,
-63.8041484437088));
#33551=CARTESIAN_POINT('Ctrl Pts',(-1.51085714423942,3.81866522988828E-5,
-63.8059282949085));
#33552=CARTESIAN_POINT('Ctrl Pts',(-1.51293366154185,5.41281456159546E-5,
-63.8079568545962));
#33553=CARTESIAN_POINT('Ctrl Pts',(-1.5151467124789,7.64762491785032E-5,
-63.8101187023241));
#33554=CARTESIAN_POINT('Ctrl Pts',(-1.51749449195499,0.000100184885069023,
-63.812412161386));
#33555=CARTESIAN_POINT('Ctrl Pts',(-1.51999108760992,0.000131146817808081,
-63.8148508937682));
#33556=CARTESIAN_POINT('Ctrl Pts',(-1.52248486630875,0.000168532538713073,
-63.8172869062401));
#33557=CARTESIAN_POINT('Ctrl Pts',(-1.52437422457671,0.000196857033155279,
-63.8191324991577));
#33558=CARTESIAN_POINT('Ctrl Pts',(-1.52626114404841,0.000228767928628635,
-63.8209757293306));
#33559=CARTESIAN_POINT('Ctrl Pts',(-1.52810370841056,0.000263295917055206,
-63.8227757579307));
#33560=CARTESIAN_POINT('Ctrl Pts',(-1.5297663700739,0.000294452691737526,
-63.8244000369018));
#33561=CARTESIAN_POINT('Ctrl Pts',(-1.53139250445785,0.000327690884682965,
-63.8259887368552));
#33562=CARTESIAN_POINT('Ctrl Pts',(-1.53298085050773,0.00036262266513698,
-63.8275407505537));
#33563=CARTESIAN_POINT('Ctrl Pts',(-1.53454774391469,0.000397082647261587,
-63.829071802324));
#33564=CARTESIAN_POINT('Ctrl Pts',(-1.53607719242315,0.000433137034783167,
-63.8305664957212));
#33565=CARTESIAN_POINT('Ctrl Pts',(-1.53760652085703,0.000471490904881078,
-63.8320614739056));
#33566=CARTESIAN_POINT('Ctrl Pts',(-1.53909804395478,0.000508896658852536,
-63.8335194958996));
#33567=CARTESIAN_POINT('Ctrl Pts',(-1.5405961355825,0.000548663598858774,
-63.8349843334466));
#33568=CARTESIAN_POINT('Ctrl Pts',(-1.54213060631517,0.000591779397113079,
-63.8364852326094));
#33569=CARTESIAN_POINT('Ctrl Pts',(-1.54377985735777,0.000638120310438484,
-63.838098400887));
#33570=CARTESIAN_POINT('Ctrl Pts',(-1.54547077478746,0.000688360290152192,
-63.8397528770161));
#33571=CARTESIAN_POINT('Ctrl Pts',(-1.54719744053054,0.000742716673563626,
-63.8414428847976));
#33572=CARTESIAN_POINT('Ctrl Pts',(-1.54917002631339,0.00080481475453534,
-63.8433735916157));
#33573=CARTESIAN_POINT('Ctrl Pts',(-1.55118873161025,0.000872336312443033,
-63.8453501484937));
#33574=CARTESIAN_POINT('Ctrl Pts',(-1.55319701397665,0.000943604228323958,
-63.8473171286807));
#33575=CARTESIAN_POINT('Ctrl Pts',(-1.55597939118099,0.00104234244754321,
-63.8500422837313));
#33576=CARTESIAN_POINT('Ctrl Pts',(-1.55873880451989,0.00114840209592754,
-63.8527461713318));
#33577=CARTESIAN_POINT('Ctrl Pts',(-1.56125854441685,0.00125139174845978,
-63.8552161386877));
#33578=CARTESIAN_POINT('Ctrl Pts',(-1.56314834933957,0.00132863398785897,
-63.8570686142046));
#33579=CARTESIAN_POINT('Ctrl Pts',(-1.56490064570691,0.00140389724196252,
-63.8587868623066));
#33580=CARTESIAN_POINT('Ctrl Pts',(-1.56643959313722,0.00147212889991266,
-63.8602963585415));
#33581=CARTESIAN_POINT('Ctrl Pts',(-1.5677289530965,0.00152929470426916,
-63.8615610437189));
#33582=CARTESIAN_POINT('Ctrl Pts',(-1.568868184354,0.00158146111032055,
-63.8626788313975));
#33583=CARTESIAN_POINT('Ctrl Pts',(-1.56983898661494,0.0016267100790277,
-63.8636316653217));
#33584=CARTESIAN_POINT('Ctrl Pts',(-1.57075171477114,0.00166925222117146,
-63.8645275000202));
#33585=CARTESIAN_POINT('Ctrl Pts',(-1.571515145023,0.00170564250684221,
-63.8652771155594));
#33586=CARTESIAN_POINT('Ctrl Pts',(-1.57214502087141,0.00173597254573887,
-63.8658958651526));
#33587=CARTESIAN_POINT('Ctrl Pts',(-1.57273209133851,0.00176424140244595,
-63.8664725654875));
#33588=CARTESIAN_POINT('Ctrl Pts',(-1.57320299278075,0.00178723762245352,
-63.8669354348749));
#33589=CARTESIAN_POINT('Ctrl Pts',(-1.57360188999628,0.00180683428705497,
-63.867327729259));
#33590=CARTESIAN_POINT('Ctrl Pts',(-1.57394979081276,0.00182392564630744,
-63.8676698713729));
#33591=CARTESIAN_POINT('Ctrl Pts',(-1.57424318974083,0.0018384486642682,
-63.8679585937126));
#33592=CARTESIAN_POINT('Ctrl Pts',(-1.57453458878625,0.00185294611160969,
-63.8682453580158));
#33593=CARTESIAN_POINT('',(-0.868245358015784,0.00185294611160958,-64.5745345887862));
#33594=CARTESIAN_POINT('Ctrl Pts',(-0.868245358015784,0.00185294611160958,
-64.5745345887862));
#33595=CARTESIAN_POINT('Ctrl Pts',(-1.10367510160594,0.00185294611160958,
-64.3391048451961));
#33596=CARTESIAN_POINT('Ctrl Pts',(-1.3391048451961,0.00185294611160958,
-64.1036751016059));
#33597=CARTESIAN_POINT('Ctrl Pts',(-1.57453458878625,0.00185294611160958,
-63.8682453580158));
#33598=CARTESIAN_POINT('',(-0.79531863640926,0.,-64.5));
#33599=CARTESIAN_POINT('Ctrl Pts',(-0.868245358015784,0.00185294611160947,
-64.5745345887863));
#33600=CARTESIAN_POINT('Ctrl Pts',(-0.867920511984305,0.00183652343213872,
-64.5742044925281));
#33601=CARTESIAN_POINT('Ctrl Pts',(-0.867592467561066,0.00182002913551296,
-64.5738711310018));
#33602=CARTESIAN_POINT('Ctrl Pts',(-0.867188603524973,0.00179989061882035,
-64.57346041281));
#33603=CARTESIAN_POINT('Ctrl Pts',(-0.866764739391085,0.00177875480534643,
-64.57302935509));
#33604=CARTESIAN_POINT('Ctrl Pts',(-0.86625756382414,0.00175361200744126,
-64.5725132968389));
#33605=CARTESIAN_POINT('Ctrl Pts',(-0.865623769120512,0.00172265954511208,
-64.5718680115171));
#33606=CARTESIAN_POINT('Ctrl Pts',(-0.864948520897705,0.00168968262836025,
-64.5711805211291));
#33607=CARTESIAN_POINT('Ctrl Pts',(-0.864129827824869,0.00165012867729293,
-64.5703466306137));
#33608=CARTESIAN_POINT('Ctrl Pts',(-0.86315671761943,0.001604232339808,
-64.5693550535868));
#33609=CARTESIAN_POINT('Ctrl Pts',(-0.862082460752306,0.00155356546215793,
-64.5682604104266));
#33610=CARTESIAN_POINT('Ctrl Pts',(-0.860820424065946,0.00149521701853039,
-64.5669740091159));
#33611=CARTESIAN_POINT('Ctrl Pts',(-0.859399706742866,0.00143187557828406,
-64.565525387959));
#33612=CARTESIAN_POINT('Ctrl Pts',(-0.857617058277222,0.00135239775434793,
-64.5637077270911));
#33613=CARTESIAN_POINT('Ctrl Pts',(-0.855585466407158,0.00126521876821512,
-64.5616355608823));
#33614=CARTESIAN_POINT('Ctrl Pts',(-0.853420628947171,0.00117763891592859,
-64.5594266767906));
#33615=CARTESIAN_POINT('Ctrl Pts',(-0.851124884258546,0.00108476312990145,
-64.5570842219804));
#33616=CARTESIAN_POINT('Ctrl Pts',(-0.848684033523705,0.000991719524374041,
-64.5545928471898));
#33617=CARTESIAN_POINT('Ctrl Pts',(-0.846246251751938,0.00090520107638592,
-64.552103587594));
#33618=CARTESIAN_POINT('Ctrl Pts',(-0.844398979277231,0.000839640184359459,
-64.5502173068831));
#33619=CARTESIAN_POINT('Ctrl Pts',(-0.842554271958467,0.000777766532134859,
-64.5483330647398));
#33620=CARTESIAN_POINT('Ctrl Pts',(-0.840753063942645,0.000720694561445301,
-64.5464926261216));
#33621=CARTESIAN_POINT('Ctrl Pts',(-0.839127695829264,0.000669194145884327,
-64.5448318572274));
#33622=CARTESIAN_POINT('Ctrl Pts',(-0.837538150811472,0.000621574660655034,
-64.543207168852));
#33623=CARTESIAN_POINT('Ctrl Pts',(-0.835985578644532,0.000577512604326147,
-64.5416197584348));
#33624=CARTESIAN_POINT('Ctrl Pts',(-0.83445351746975,0.00053403265072395,
-64.540053319257));
#33625=CARTESIAN_POINT('Ctrl Pts',(-0.832958118217025,0.000493996445435221,
-64.5385238533706));
#33626=CARTESIAN_POINT('Ctrl Pts',(-0.831462700584247,0.000456253937660245,
-64.5369939676883));
#33627=CARTESIAN_POINT('Ctrl Pts',(-0.830004714201859,0.000419456148757018,
-64.5355023760136));
#33628=CARTESIAN_POINT('Ctrl Pts',(-0.828540166631002,0.000384680303812991,
-64.5340037037557));
#33629=CARTESIAN_POINT('Ctrl Pts',(-0.827039815786342,0.000351435419327029,
-64.5324681805947));
#33630=CARTESIAN_POINT('Ctrl Pts',(-0.825427211040693,0.000315703204637751,
-64.530817771995));
#33631=CARTESIAN_POINT('Ctrl Pts',(-0.823773595132572,0.000281787957708217,
-64.529125149268));
#33632=CARTESIAN_POINT('Ctrl Pts',(-0.822084705002914,0.000250206967384647,
-64.5273963190708));
#33633=CARTESIAN_POINT('Ctrl Pts',(-0.820155155817438,0.00021412583156339,
-64.5254211385423));
#33634=CARTESIAN_POINT('Ctrl Pts',(-0.818180086158876,0.000181169469766856,
-64.5233992312895));
#33635=CARTESIAN_POINT('Ctrl Pts',(-0.816214827518119,0.000152480845410752,
-64.5213873627599));
#33636=CARTESIAN_POINT('Ctrl Pts',(-0.813492568573185,0.000112741615850007,
-64.5186005402078));
#33637=CARTESIAN_POINT('Ctrl Pts',(-0.810792018065188,8.14691463192202E-5,
-64.5158359360067));
#33638=CARTESIAN_POINT('Ctrl Pts',(-0.808325391140352,5.90616066569183E-5,
-64.5133109478137));
#33639=CARTESIAN_POINT('Ctrl Pts',(-0.806475420946726,4.22559519101918E-5,
-64.5114172066688));
#33640=CARTESIAN_POINT('Ctrl Pts',(-0.804759675671119,3.03183594525773E-5,
-64.5096609508553));
#33641=CARTESIAN_POINT('Ctrl Pts',(-0.803252515255964,2.19691435532354E-5,
-64.5081183094309));
#33642=CARTESIAN_POINT('Ctrl Pts',(-0.801989757154794,1.49738430468668E-5,
-64.5068258239488));
#33643=CARTESIAN_POINT('Ctrl Pts',(-0.800873785775093,1.04521897691688E-5,
-64.5056836631396));
#33644=CARTESIAN_POINT('Ctrl Pts',(-0.799922600320211,7.39546431272053E-6,
-64.5047102375997));
#33645=CARTESIAN_POINT('Ctrl Pts',(-0.799028303767072,4.52155678442164E-6,
-64.5037950311059));
#33646=CARTESIAN_POINT('Ctrl Pts',(-0.798280081319924,2.92603171309864E-6,
-64.5030293988184));
#33647=CARTESIAN_POINT('Ctrl Pts',(-0.797662574868972,1.91616332645417E-6,
-64.5023976001144));
#33648=CARTESIAN_POINT('Ctrl Pts',(-0.797087026101143,9.74912421775467E-7,
-64.5018087302087));
#33649=CARTESIAN_POINT('Ctrl Pts',(-0.796625180682792,5.41797940511647E-7,
-64.5013362750361));
#33650=CARTESIAN_POINT('Ctrl Pts',(-0.796233819415205,2.9201856199812E-7,
-64.500935978419));
#33651=CARTESIAN_POINT('Ctrl Pts',(-0.795892553137518,7.42114211081106E-8,
-64.5005869205336));
#33652=CARTESIAN_POINT('Ctrl Pts',(-0.795604617783312,-2.22022958507712E-16,
-64.5002924603909));
#33653=CARTESIAN_POINT('Ctrl Pts',(-0.79531863640926,-2.22044604925031E-16,
-64.5));
#33654=CARTESIAN_POINT('',(-1.14765931820463,0.,-64.1476593182046));
#33655=CARTESIAN_POINT('Ctrl Pts',(-0.868245358015784,0.00185294611160958,
-64.5745345887862));
#33656=CARTESIAN_POINT('Ctrl Pts',(-1.24643975969902,0.0209726669473527,
-64.9588414442702));
#33657=CARTESIAN_POINT('Ctrl Pts',(-1.89279714334289,0.308835349231178,
-65.5507400778319));
#33658=CARTESIAN_POINT('Ctrl Pts',(-2.42122743991223,0.985650418224739,
-65.9509027104217));
#33659=CARTESIAN_POINT('Ctrl Pts',(-2.49999999999999,1.33275179473161,-66.));
#33660=CARTESIAN_POINT('Ctrl Pts',(-2.49999999999999,1.5,-66.));
#33661=CARTESIAN_POINT('Ctrl Pts',(-1.10367510160594,0.00185294611160958,
-64.3391048451961));
#33662=CARTESIAN_POINT('Ctrl Pts',(-1.48390698788943,0.020972666947353,
-64.7213742160798));
#33663=CARTESIAN_POINT('Ctrl Pts',(-2.11211145483922,0.308835349231178,
-65.3314257663356));
#33664=CARTESIAN_POINT('Ctrl Pts',(-2.59778586341538,0.985650418224741,
-65.7743442869185));
#33665=CARTESIAN_POINT('Ctrl Pts',(-2.66666666666666,1.33275179473161,-65.8333333333333));
#33666=CARTESIAN_POINT('Ctrl Pts',(-2.66666666666666,1.5,-65.8333333333333));
#33667=CARTESIAN_POINT('Ctrl Pts',(-1.3391048451961,0.00185294611160958,
-64.1036751016059));
#33668=CARTESIAN_POINT('Ctrl Pts',(-1.72137421607983,0.0209726669473534,
-64.4839069878894));
#33669=CARTESIAN_POINT('Ctrl Pts',(-2.33142576633555,0.308835349231176,
-65.1121114548392));
#33670=CARTESIAN_POINT('Ctrl Pts',(-2.77434428691853,0.985650418224743,
-65.5977858634154));
#33671=CARTESIAN_POINT('Ctrl Pts',(-2.83333333333333,1.33275179473161,-65.6666666666667));
#33672=CARTESIAN_POINT('Ctrl Pts',(-2.83333333333333,1.5,-65.6666666666667));
#33673=CARTESIAN_POINT('Ctrl Pts',(-1.57453458878625,0.00185294611160958,
-63.8682453580158));
#33674=CARTESIAN_POINT('Ctrl Pts',(-1.95884144427023,0.0209726669473537,
-64.246439759699));
#33675=CARTESIAN_POINT('Ctrl Pts',(-2.55074007783188,0.308835349231176,
-64.8927971433429));
#33676=CARTESIAN_POINT('Ctrl Pts',(-2.95090271042168,0.985650418224745,
-65.4212274399123));
#33677=CARTESIAN_POINT('Ctrl Pts',(-3.,1.33275179473161,-65.5));
#33678=CARTESIAN_POINT('Ctrl Pts',(-3.,1.5,-65.5));
#33679=CARTESIAN_POINT('',(-3.,1.5,-65.5));
#33680=CARTESIAN_POINT('Ctrl Pts',(-1.57453458878625,0.00185294611160958,
-63.8682453580158));
#33681=CARTESIAN_POINT('Ctrl Pts',(-1.95884144427023,0.0209726669473537,
-64.246439759699));
#33682=CARTESIAN_POINT('Ctrl Pts',(-2.55074007783188,0.308835349231176,
-64.8927971433429));
#33683=CARTESIAN_POINT('Ctrl Pts',(-2.95090271042168,0.985650418224745,
-65.4212274399123));
#33684=CARTESIAN_POINT('Ctrl Pts',(-3.,1.33275179473161,-65.5));
#33685=CARTESIAN_POINT('Ctrl Pts',(-3.,1.5,-65.5));
#33686=CARTESIAN_POINT('',(-2.49999999999999,1.5,-66.));
#33687=CARTESIAN_POINT('',(-3.,1.5,-65.5));
#33688=CARTESIAN_POINT('Ctrl Pts',(-2.49999999999999,1.5,-66.));
#33689=CARTESIAN_POINT('Ctrl Pts',(-2.49999999999999,1.33275179473161,-66.));
#33690=CARTESIAN_POINT('Ctrl Pts',(-2.42122743991223,0.985650418224739,
-65.9509027104217));
#33691=CARTESIAN_POINT('Ctrl Pts',(-1.89279714334289,0.308835349231178,
-65.5507400778319));
#33692=CARTESIAN_POINT('Ctrl Pts',(-1.24643975969902,0.0209726669473527,
-64.9588414442702));
#33693=CARTESIAN_POINT('Ctrl Pts',(-0.868245358015784,0.00185294611160958,
-64.5745345887862));
#33694=CARTESIAN_POINT('Origin',(-2.75,4.,-65.75));
#33695=CARTESIAN_POINT('',(-3.,4.,-65.5));
#33696=CARTESIAN_POINT('',(-2.5,4.,-66.));
#33697=CARTESIAN_POINT('',(-14.375,4.,-54.125));
#33698=CARTESIAN_POINT('',(-2.5,4.,-66.));
#33699=CARTESIAN_POINT('',(-3.,4.,-65.5));
#33700=CARTESIAN_POINT('Origin',(0.,0.,-16.5));
#33701=CARTESIAN_POINT('',(-38.,0.,42.));
#33702=CARTESIAN_POINT('',(-17.5,0.,42.));
#33703=CARTESIAN_POINT('',(-19.,0.,42.));
#33704=CARTESIAN_POINT('',(-64.5,0.,15.5));
#33705=CARTESIAN_POINT('Origin',(-38.,0.,15.5));
#33706=CARTESIAN_POINT('',(-64.5,0.,-48.5));
#33707=CARTESIAN_POINT('',(-64.5,0.,-32.5));
#33708=CARTESIAN_POINT('',(-38.,0.,-75.));
#33709=CARTESIAN_POINT('Origin',(-38.,0.,-48.5));
#33710=CARTESIAN_POINT('',(38.,0.,-75.));
#33711=CARTESIAN_POINT('',(19.,0.,-75.));
#33712=CARTESIAN_POINT('',(64.5,0.,-48.5));
#33713=CARTESIAN_POINT('Origin',(38.,0.,-48.5));
#33714=CARTESIAN_POINT('',(64.5,0.,15.5));
#33715=CARTESIAN_POINT('',(64.5,0.,-0.500000000000003));
#33716=CARTESIAN_POINT('',(38.,0.,42.));
#33717=CARTESIAN_POINT('Origin',(38.,0.,15.5));
#33718=CARTESIAN_POINT('',(17.5,0.,42.));
#33719=CARTESIAN_POINT('',(-19.,0.,42.));
#33720=CARTESIAN_POINT('Origin',(0.,0.,0.));
#33721=CARTESIAN_POINT('',(47.2,0.,-7.34788079488411E-16));
#33722=CARTESIAN_POINT('Origin',(53.2,0.,0.));
#33723=CARTESIAN_POINT('',(0.795318636409267,0.,-64.5));
#33724=CARTESIAN_POINT('',(-1.5,0.,-64.5));
#33725=CARTESIAN_POINT('',(1.5,0.,-63.7953186364093));
#33726=CARTESIAN_POINT('',(1.14765931820464,0.,-64.1476593182046));
#33727=CARTESIAN_POINT('',(1.50000000000001,0.,-45.4752680036083));
#33728=CARTESIAN_POINT('',(1.5,0.,-41.25));
#33729=CARTESIAN_POINT('',(31.0952102098472,0.,-33.2165305534069));
#33730=CARTESIAN_POINT('Origin',(0.,0.,0.));
#33731=CARTESIAN_POINT('',(45.2548339959391,0.,-47.3761543394987));
#33732=CARTESIAN_POINT('',(18.6206890143242,0.,-20.7420093578839));
#33733=CARTESIAN_POINT('',(47.3761543394987,0.,-45.254833995939));
#33734=CARTESIAN_POINT('',(41.129833995939,0.,-51.5011543394987));
#33735=CARTESIAN_POINT('',(33.2165305534069,0.,-31.0952102098472));
#33736=CARTESIAN_POINT('',(28.5201839509359,0.,-26.3988636073762));
#33737=CARTESIAN_POINT('',(45.209022556391,0.,-5.13753632549022));
#33738=CARTESIAN_POINT('Origin',(0.,0.,0.));
#33739=CARTESIAN_POINT('',(59.5,0.,-7.11055553385247));
#33740=CARTESIAN_POINT('Origin',(53.2,0.,0.));
#33741=CARTESIAN_POINT('',(59.5,0.,-46.5));
#33742=CARTESIAN_POINT('',(59.5,0.,-1.5));
#33743=CARTESIAN_POINT('',(36.,0.,-70.));
#33744=CARTESIAN_POINT('Origin',(36.,0.,-46.5));
#33745=CARTESIAN_POINT('',(-36.,0.,-70.));
#33746=CARTESIAN_POINT('',(18.,0.,-70.));
#33747=CARTESIAN_POINT('',(-59.5,0.,-46.5));
#33748=CARTESIAN_POINT('Origin',(-36.,0.,-46.5));
#33749=CARTESIAN_POINT('',(-59.5,0.,-7.11055553385247));
#33750=CARTESIAN_POINT('',(-59.5,0.,-31.5));
#33751=CARTESIAN_POINT('',(-45.209022556391,0.,-5.13753632549022));
#33752=CARTESIAN_POINT('Origin',(-53.2,0.,0.));
#33753=CARTESIAN_POINT('',(-33.2165305534069,0.,-31.0952102098472));
#33754=CARTESIAN_POINT('Origin',(0.,0.,0.));
#33755=CARTESIAN_POINT('',(-46.1707625875413,0.,-44.0494422439817));
#33756=CARTESIAN_POINT('',(-20.7420093578839,0.,-18.6206890143242));
#33757=CARTESIAN_POINT('',(-46.1707625875413,0.,-45.0460121855233));
#33758=CARTESIAN_POINT('',(-46.1707625875413,0.,-44.5477272147525));
#33759=CARTESIAN_POINT('',(-45.0460121855233,0.,-46.1707625875413));
#33760=CARTESIAN_POINT('',(-42.5440475583121,0.,-48.6727272147525));
#33761=CARTESIAN_POINT('',(-44.0494422439817,0.,-46.1707625875413));
#33762=CARTESIAN_POINT('',(-44.5477272147525,0.,-46.1707625875413));
#33763=CARTESIAN_POINT('',(-31.0952102098472,0.,-33.2165305534069));
#33764=CARTESIAN_POINT('',(-26.3988636073762,0.,-28.5201839509359));
#33765=CARTESIAN_POINT('',(-1.49999999999998,0.,-45.4752680036083));
#33766=CARTESIAN_POINT('Origin',(0.,0.,0.));
#33767=CARTESIAN_POINT('',(-1.5,0.,-30.25));
#33768=CARTESIAN_POINT('',(59.5,0.,13.5));
#33769=CARTESIAN_POINT('',(36.,0.,37.));
#33770=CARTESIAN_POINT('Origin',(36.,0.,13.5));
#33771=CARTESIAN_POINT('',(59.5,0.,7.11055553385247));
#33772=CARTESIAN_POINT('',(59.5,0.,-1.5));
#33773=CARTESIAN_POINT('',(45.209022556391,0.,5.13753632549028));
#33774=CARTESIAN_POINT('Origin',(53.2,0.,0.));
#33775=CARTESIAN_POINT('',(26.4811253537307,0.,37.));
#33776=CARTESIAN_POINT('Origin',(0.,0.,0.));
#33777=CARTESIAN_POINT('',(-18.,0.,37.));
#33778=CARTESIAN_POINT('',(36.4780836837786,0.,19.3232453474888));
#33779=CARTESIAN_POINT('',(29.8463073008423,0.,28.5172989692869));
#33780=CARTESIAN_POINT('Origin',(30.5,0.,22.));
#33781=CARTESIAN_POINT('',(-5.05534198688027E-15,0.,-41.28));
#33782=CARTESIAN_POINT('Origin',(0.,0.,0.));
#33783=CARTESIAN_POINT('',(-36.4780836837786,0.,19.3232453474888));
#33784=CARTESIAN_POINT('Origin',(0.,0.,0.));
#33785=CARTESIAN_POINT('',(-29.8463073008423,0.,28.5172989692869));
#33786=CARTESIAN_POINT('Origin',(-30.5,0.,22.));
#33787=CARTESIAN_POINT('Origin',(0.,0.,0.));
#33788=CARTESIAN_POINT('',(-36.,0.,37.));
#33789=CARTESIAN_POINT('',(-59.5,0.,13.5));
#33790=CARTESIAN_POINT('Origin',(-36.,0.,13.5));
#33791=CARTESIAN_POINT('',(-26.4811253537307,0.,37.));
#33792=CARTESIAN_POINT('',(-18.,0.,37.));
#33793=CARTESIAN_POINT('',(-45.209022556391,0.,5.13753632549025));
#33794=CARTESIAN_POINT('Origin',(0.,0.,0.));
#33795=CARTESIAN_POINT('',(-59.5,0.,7.11055553385247));
#33796=CARTESIAN_POINT('Origin',(-53.2,0.,0.));
#33797=CARTESIAN_POINT('',(-59.5,0.,-31.5));
#33798=CARTESIAN_POINT('',(-59.2,0.,-7.34788079488411E-16));
#33799=CARTESIAN_POINT('Origin',(-53.2,0.,0.));
#33800=CARTESIAN_POINT('Origin',(-1.5,1.5,-64.5));
#33801=CARTESIAN_POINT('',(2.5,1.5,-66.));
#33802=CARTESIAN_POINT('',(-1.5,1.5,-66.));
#33803=CARTESIAN_POINT('',(0.868245358015795,0.00185294611160958,-64.5745345887862));
#33804=CARTESIAN_POINT('Ctrl Pts',(0.868245358015795,0.00185294611160958,
-64.5745345887862));
#33805=CARTESIAN_POINT('Ctrl Pts',(1.12037495913795,0.0145994266687717,
-64.8307391591089));
#33806=CARTESIAN_POINT('Ctrl Pts',(1.63375136411347,0.173220581778977,-65.3201513636217));
#33807=CARTESIAN_POINT('Ctrl Pts',(2.13540546748456,0.600909021307247,-65.7357961587963));
#33808=CARTESIAN_POINT('Ctrl Pts',(2.43900967406247,1.07263972227481,-65.9615334712268));
#33809=CARTESIAN_POINT('Ctrl Pts',(2.5,1.33275179473161,-66.));
#33810=CARTESIAN_POINT('Ctrl Pts',(2.5,1.5,-66.));
#33811=CARTESIAN_POINT('Ctrl Pts',(0.795318636409267,-2.22044604925031E-16,
-64.5));
#33812=CARTESIAN_POINT('Ctrl Pts',(0.795642656641266,-2.22020079281761E-16,
-64.5003313610337));
#33813=CARTESIAN_POINT('Ctrl Pts',(0.795969871010492,9.12216844667872E-8,
-64.5006659910395));
#33814=CARTESIAN_POINT('Ctrl Pts',(0.796372819533867,3.87472611551587E-7,
-64.5010781547591));
#33815=CARTESIAN_POINT('Ctrl Pts',(0.79679572105221,6.98393137642135E-7,
-64.501510727787));
#33816=CARTESIAN_POINT('Ctrl Pts',(0.797301839401443,1.2319450398306E-6,
-64.5020284953742));
#33817=CARTESIAN_POINT('Ctrl Pts',(0.797934442187392,2.38657547613208E-6,
-64.502675765448));
#33818=CARTESIAN_POINT('Ctrl Pts',(0.798608415722088,3.61671605360927E-6,
-64.5033653654769));
#33819=CARTESIAN_POINT('Ctrl Pts',(0.799425679468639,5.55516755123648E-6,
-64.5042016754148));
#33820=CARTESIAN_POINT('Ctrl Pts',(0.800397213439585,8.99934440856676E-6,
-64.505195955373));
#33821=CARTESIAN_POINT('Ctrl Pts',(0.801469705844418,1.28014281553561E-5,
-64.5062935574489));
#33822=CARTESIAN_POINT('Ctrl Pts',(0.802729790879233,1.84658046873067E-5,
-64.5075832522893));
#33823=CARTESIAN_POINT('Ctrl Pts',(0.804148443709076,2.72127176239589E-5,
-64.5090353424031));
#33824=CARTESIAN_POINT('Ctrl Pts',(0.805928294908851,3.81866523013816E-5,
-64.5108571442398));
#33825=CARTESIAN_POINT('Ctrl Pts',(0.807956854596668,5.41281456196828E-5,
-64.5129336615424));
#33826=CARTESIAN_POINT('Ctrl Pts',(0.810118702324731,7.64762491842763E-5,
-64.5151467124795));
#33827=CARTESIAN_POINT('Ctrl Pts',(0.812412161386584,0.000100184885074821,
-64.5174944919555));
#33828=CARTESIAN_POINT('Ctrl Pts',(0.814850893768659,0.000131146817813719,
-64.5199910876103));
#33829=CARTESIAN_POINT('Ctrl Pts',(0.817286906240445,0.000168532538717292,
-64.522484866309));
#33830=CARTESIAN_POINT('Ctrl Pts',(0.819132499158045,0.000196857033159806,
-64.524374224577));
#33831=CARTESIAN_POINT('Ctrl Pts',(0.82097572933093,0.000228767928633297,
-64.5262611440487));
#33832=CARTESIAN_POINT('Ctrl Pts',(0.82277575793104,0.000263295917060091,
-64.5281037084108));
#33833=CARTESIAN_POINT('Ctrl Pts',(0.824400036902089,0.000294452691741817,
-64.5297663700741));
#33834=CARTESIAN_POINT('Ctrl Pts',(0.82598873685544,0.000327690884686428,
-64.531392504458));
#33835=CARTESIAN_POINT('Ctrl Pts',(0.827540750553837,0.000362622665139645,
-64.5329808505079));
#33836=CARTESIAN_POINT('Ctrl Pts',(0.82907180232416,0.000397082647263948,
-64.5345477439148));
#33837=CARTESIAN_POINT('Ctrl Pts',(0.830566495721296,0.000433137034785286,
-64.5360771924232));
#33838=CARTESIAN_POINT('Ctrl Pts',(0.832061473905696,0.000471490904882854,
-64.5376065208571));
#33839=CARTESIAN_POINT('Ctrl Pts',(0.833519495899744,0.000508896658854833,
-64.5390980439549));
#33840=CARTESIAN_POINT('Ctrl Pts',(0.834984333446768,0.000548663598861856,
-64.5405961355826));
#33841=CARTESIAN_POINT('Ctrl Pts',(0.836485232609497,0.000591779397116854,
-64.5421306063153));
#33842=CARTESIAN_POINT('Ctrl Pts',(0.838098400887085,0.000638120310440689,
-64.5437798573578));
#33843=CARTESIAN_POINT('Ctrl Pts',(0.839752877016141,0.000688360290152621,
-64.5454707747875));
#33844=CARTESIAN_POINT('Ctrl Pts',(0.841442884797579,0.00074271667356185,
-64.5471974405305));
#33845=CARTESIAN_POINT('Ctrl Pts',(0.843373591615611,0.000804814754531903,
-64.5491700263133));
#33846=CARTESIAN_POINT('Ctrl Pts',(0.845350148493538,0.000872336312437336,
-64.5511887316101));
#33847=CARTESIAN_POINT('Ctrl Pts',(0.847317128680503,0.000943604228316186,
-64.5531970139764));
#33848=CARTESIAN_POINT('Ctrl Pts',(0.850042283731077,0.00104234244753579,
-64.5559793911808));
#33849=CARTESIAN_POINT('Ctrl Pts',(0.852746171331635,0.00114840209592096,
-64.5587388045197));
#33850=CARTESIAN_POINT('Ctrl Pts',(0.855216138687543,0.00125139174845401,
-64.5612585444167));
#33851=CARTESIAN_POINT('Ctrl Pts',(0.857068614204475,0.0013286339878538,
-64.5631483493395));
#33852=CARTESIAN_POINT('Ctrl Pts',(0.858786862306446,0.00140389724195783,
-64.5649006457068));
#33853=CARTESIAN_POINT('Ctrl Pts',(0.860296358541392,0.00147212889990866,
-64.5664395931371));
#33854=CARTESIAN_POINT('Ctrl Pts',(0.861561043718845,0.00152929470426492,
-64.5677289530964));
#33855=CARTESIAN_POINT('Ctrl Pts',(0.862678831397432,0.00158146111031607,
-64.5688681843539));
#33856=CARTESIAN_POINT('Ctrl Pts',(0.863631665321587,0.00162671007902326,
-64.5698389866149));
#33857=CARTESIAN_POINT('Ctrl Pts',(0.864527500020132,0.00166925222116752,
-64.5707517147711));
#33858=CARTESIAN_POINT('Ctrl Pts',(0.865277115559362,0.00170564250683912,
-64.5715151450229));
#33859=CARTESIAN_POINT('Ctrl Pts',(0.865895865152574,0.00173597254573621,
-64.5721450208714));
#33860=CARTESIAN_POINT('Ctrl Pts',(0.866472565487434,0.00176424140244366,
-64.5727320913385));
#33861=CARTESIAN_POINT('Ctrl Pts',(0.866935434874884,0.00178723762245152,
-64.5732029927807));
#33862=CARTESIAN_POINT('Ctrl Pts',(0.867327729258992,0.00180683428705319,
-64.5736018899962));
#33863=CARTESIAN_POINT('Ctrl Pts',(0.867669871372873,0.00182392564630644,
-64.5739497908127));
#33864=CARTESIAN_POINT('Ctrl Pts',(0.867958593712563,0.00183844866426747,
-64.5742431897408));
#33865=CARTESIAN_POINT('Ctrl Pts',(0.868245358015795,0.00185294611160947,
-64.5745345887863));
#33866=CARTESIAN_POINT('Origin',(-3.,4.,-66.));
#33867=CARTESIAN_POINT('',(2.5,4.,-66.));
#33868=CARTESIAN_POINT('',(-1.5,4.,-66.));
#33869=CARTESIAN_POINT('',(2.5,4.,-66.));
#33870=CARTESIAN_POINT('Ctrl Pts',(0.868245358015795,0.00185294611160958,
-64.5745345887862));
#33871=CARTESIAN_POINT('Ctrl Pts',(0.864163358505955,0.00164657951619623,
-64.5703866151813));
#33872=CARTESIAN_POINT('Ctrl Pts',(0.834260393339435,0.000219540540015439,
-64.539887259118));
#33873=CARTESIAN_POINT('Ctrl Pts',(0.801608171182561,1.28888202263847E-5,
-64.5064246347597));
#33874=CARTESIAN_POINT('Ctrl Pts',(0.796336597880222,9.63140470631229E-20,
-64.5010410237755));
#33875=CARTESIAN_POINT('Ctrl Pts',(0.795318636409267,0.,-64.5));
#33876=CARTESIAN_POINT('Ctrl Pts',(1.10367510160595,0.00185294611160967,
-64.3391048451961));
#33877=CARTESIAN_POINT('Ctrl Pts',(1.09957111073108,0.0016465795161963,
-64.3349788629562));
#33878=CARTESIAN_POINT('Ctrl Pts',(1.06943670599212,0.000219540540015618,
-64.3047109464653));
#33879=CARTESIAN_POINT('Ctrl Pts',(1.03655657695391,1.28888202263034E-5,
-64.2714762289883));
#33880=CARTESIAN_POINT('Ctrl Pts',(1.03123807317865,2.26183380401734E-19,
-64.2661395484771));
#33881=CARTESIAN_POINT('Ctrl Pts',(1.03021242427285,0.,-64.2651062121364));
#33882=CARTESIAN_POINT('Ctrl Pts',(1.33910484519611,0.00185294611160976,
-64.1036751016059));
#33883=CARTESIAN_POINT('Ctrl Pts',(1.33497886295621,0.0016465795161964,
-64.0995711107311));
#33884=CARTESIAN_POINT('Ctrl Pts',(1.30453395202334,-2.1594682714537E-5,
-64.0694367059921));
#33885=CARTESIAN_POINT('Ctrl Pts',(1.27145164420996,0.000165305522379591,
-64.0365565769539));
#33886=CARTESIAN_POINT('Ctrl Pts',(1.26613954847709,3.59888273472094E-19,
-64.0312380731786));
#33887=CARTESIAN_POINT('Ctrl Pts',(1.26510621213642,0.,-64.0302124242728));
#33888=CARTESIAN_POINT('Ctrl Pts',(1.57453458878627,0.00185294611160985,
-63.8682453580158));
#33889=CARTESIAN_POINT('Ctrl Pts',(1.57038661518134,0.0016465795161965,
-63.8641633585059));
#33890=CARTESIAN_POINT('Ctrl Pts',(1.539887259118,0.000219540540015942,
-63.8342603933394));
#33891=CARTESIAN_POINT('Ctrl Pts',(1.5064246347597,1.28888202263958E-5,
-63.8016081711826));
#33892=CARTESIAN_POINT('Ctrl Pts',(1.50104102377552,4.81570235315835E-19,
-63.7963365978802));
#33893=CARTESIAN_POINT('Ctrl Pts',(1.5,0.,-63.7953186364093));
#33894=CARTESIAN_POINT('',(1.57453458878627,0.00185294611160985,-63.8682453580158));
#33895=CARTESIAN_POINT('Ctrl Pts',(1.57453458878627,0.00185294611160985,
-63.8682453580158));
#33896=CARTESIAN_POINT('Ctrl Pts',(1.33910484519611,0.00185294611160976,
-64.1036751016059));
#33897=CARTESIAN_POINT('Ctrl Pts',(1.10367510160595,0.00185294611160967,
-64.3391048451961));
#33898=CARTESIAN_POINT('Ctrl Pts',(0.868245358015795,0.00185294611160958,
-64.5745345887862));
#33899=CARTESIAN_POINT('Ctrl Pts',(1.57453458878627,0.00185294611160969,
-63.8682453580158));
#33900=CARTESIAN_POINT('Ctrl Pts',(1.57420449252805,0.00183652343213895,
-63.8679205119843));
#33901=CARTESIAN_POINT('Ctrl Pts',(1.57387113100176,0.00182002913551295,
-63.8675924675611));
#33902=CARTESIAN_POINT('Ctrl Pts',(1.57346041281005,0.00179989061882035,
-63.867188603525));
#33903=CARTESIAN_POINT('Ctrl Pts',(1.57302935509002,0.0017787548053465,
-63.8667647393911));
#33904=CARTESIAN_POINT('Ctrl Pts',(1.57251329683896,0.00175361200744156,
-63.8662575638241));
#33905=CARTESIAN_POINT('Ctrl Pts',(1.57186801151716,0.00172265954511253,
-63.8656237691205));
#33906=CARTESIAN_POINT('Ctrl Pts',(1.57118052112909,0.00168968262836032,
-63.8649485208977));
#33907=CARTESIAN_POINT('Ctrl Pts',(1.5703466306137,0.0016501286772923,-63.8641298278249));
#33908=CARTESIAN_POINT('Ctrl Pts',(1.56935505358675,0.00160423233980667,
-63.8631567176194));
#33909=CARTESIAN_POINT('Ctrl Pts',(1.56826041042658,0.00155356546215597,
-63.8620824607523));
#33910=CARTESIAN_POINT('Ctrl Pts',(1.56697400911583,0.00149521701852808,
-63.8608204240659));
#33911=CARTESIAN_POINT('Ctrl Pts',(1.56552538795896,0.00143187557828095,
-63.8593997067428));
#33912=CARTESIAN_POINT('Ctrl Pts',(1.56370772709104,0.00135239775434526,
-63.8576170582771));
#33913=CARTESIAN_POINT('Ctrl Pts',(1.56163556088225,0.0012652187682126,
-63.8555854664071));
#33914=CARTESIAN_POINT('Ctrl Pts',(1.55942667679053,0.00117763891592682,
-63.8534206289471));
#33915=CARTESIAN_POINT('Ctrl Pts',(1.55708422198041,0.00108476312990192,
-63.8511248842586));
#33916=CARTESIAN_POINT('Ctrl Pts',(1.55459284718984,0.000991719524377037,
-63.8486840335238));
#33917=CARTESIAN_POINT('Ctrl Pts',(1.55210358759418,0.000905201076390805,
-63.8462462517521));
#33918=CARTESIAN_POINT('Ctrl Pts',(1.55021730688321,0.000839640184363255,
-63.8443989792773));
#33919=CARTESIAN_POINT('Ctrl Pts',(1.54833306473991,0.000777766532137521,
-63.8425542719585));
#33920=CARTESIAN_POINT('Ctrl Pts',(1.54649262612169,0.000720694561447077,
-63.8407530639427));
#33921=CARTESIAN_POINT('Ctrl Pts',(1.54483185722751,0.000669194145886256,
-63.8391276958293));
#33922=CARTESIAN_POINT('Ctrl Pts',(1.54320716885208,0.000621574660657379,
-63.8375381508115));
#33923=CARTESIAN_POINT('Ctrl Pts',(1.54161975843489,0.000577512604328589,
-63.8359855786446));
#33924=CARTESIAN_POINT('Ctrl Pts',(1.54005331925714,0.000534032650727231,
-63.8344535174698));
#33925=CARTESIAN_POINT('Ctrl Pts',(1.53852385337071,0.000493996445439231,
-63.8329581182172));
#33926=CARTESIAN_POINT('Ctrl Pts',(1.53699396768853,0.000456253937664908,
-63.8314627005844));
#33927=CARTESIAN_POINT('Ctrl Pts',(1.53550237601382,0.000419456148761565,
-63.830004714202));
#33928=CARTESIAN_POINT('Ctrl Pts',(1.53400370375587,0.000384680303817308,
-63.8285401666312));
#33929=CARTESIAN_POINT('Ctrl Pts',(1.53246818059487,0.000351435419331247,
-63.8270398157865));
#33930=CARTESIAN_POINT('Ctrl Pts',(1.53081777199523,0.000315703204641898,
-63.8254272110409));
#33931=CARTESIAN_POINT('Ctrl Pts',(1.52912514926818,0.000281787957712134,
-63.8237735951328));
#33932=CARTESIAN_POINT('Ctrl Pts',(1.52739631907099,0.000250206967388422,
-63.8220847050031));
#33933=CARTESIAN_POINT('Ctrl Pts',(1.52542113854251,0.000214125831566566,
-63.8201551558176));
#33934=CARTESIAN_POINT('Ctrl Pts',(1.52339923128973,0.00018116946976938,
-63.818180086159));
#33935=CARTESIAN_POINT('Ctrl Pts',(1.52138736276008,0.00015248084541275,
-63.8162148275183));
#33936=CARTESIAN_POINT('Ctrl Pts',(1.51860054020794,0.000112741615851503,
-63.8134925685733));
#33937=CARTESIAN_POINT('Ctrl Pts',(1.51583593600687,8.14691463204668E-5,
-63.8107920180653));
#33938=CARTESIAN_POINT('Ctrl Pts',(1.51331094781377,5.90616066578065E-5,
-63.8083253911404));
#33939=CARTESIAN_POINT('Ctrl Pts',(1.51141720666895,4.22559519108112E-5,
-63.8064754209468));
#33940=CARTESIAN_POINT('Ctrl Pts',(1.50966095085537,3.03183594527219E-5,
-63.8047596756712));
#33941=CARTESIAN_POINT('Ctrl Pts',(1.50811830943101,2.19691435532354E-5,
-63.803252515256));
#33942=CARTESIAN_POINT('Ctrl Pts',(1.50682582394888,1.49738430467655E-5,
-63.8019897571548));
#33943=CARTESIAN_POINT('Ctrl Pts',(1.5056836631397,1.04521897692208E-5,
-63.8008737857751));
#33944=CARTESIAN_POINT('Ctrl Pts',(1.50471023759975,7.39546431272053E-6,
-63.7999226003202));
#33945=CARTESIAN_POINT('Ctrl Pts',(1.50379503110595,4.521556784394E-6,-63.7990283037671));
#33946=CARTESIAN_POINT('Ctrl Pts',(1.50302939881844,2.92603171356413E-6,
-63.79828008132));
#33947=CARTESIAN_POINT('Ctrl Pts',(1.50239760011449,1.91616332689826E-6,
-63.797662574869));
#33948=CARTESIAN_POINT('Ctrl Pts',(1.50180873020872,9.74912422190382E-7,
-63.7970870261012));
#33949=CARTESIAN_POINT('Ctrl Pts',(1.50133627503617,5.41797940298606E-7,
-63.7966251806828));
#33950=CARTESIAN_POINT('Ctrl Pts',(1.50093597841904,2.92018561776075E-7,
-63.7962338194152));
#33951=CARTESIAN_POINT('Ctrl Pts',(1.50058692053362,7.42114208744582E-8,
-63.7958925531375));
#33952=CARTESIAN_POINT('Ctrl Pts',(1.50029246039094,-2.2193637283843E-16,
-63.7956046177833));
#33953=CARTESIAN_POINT('Ctrl Pts',(1.5,-2.22044604925031E-16,-63.7953186364093));
#33954=CARTESIAN_POINT('Ctrl Pts',(1.57453458878627,0.00185294611160985,
-63.8682453580158));
#33955=CARTESIAN_POINT('Ctrl Pts',(1.83073915910892,0.0145994266687731,
-64.1203749591379));
#33956=CARTESIAN_POINT('Ctrl Pts',(2.32015136362177,0.173220581778977,-64.6337513641135));
#33957=CARTESIAN_POINT('Ctrl Pts',(2.73579615879626,0.600909021307247,-65.1354054674845));
#33958=CARTESIAN_POINT('Ctrl Pts',(2.96153347122678,1.07263972227482,-65.4390096740624));
#33959=CARTESIAN_POINT('Ctrl Pts',(3.,1.33275179473161,-65.5));
#33960=CARTESIAN_POINT('Ctrl Pts',(3.,1.5,-65.5));
#33961=CARTESIAN_POINT('Ctrl Pts',(1.33910484519611,0.00185294611160976,
-64.1036751016059));
#33962=CARTESIAN_POINT('Ctrl Pts',(1.59395109245193,0.0145994266687726,
-64.3571630257949));
#33963=CARTESIAN_POINT('Ctrl Pts',(2.09135136378567,0.173220581778977,-64.8625513639496));
#33964=CARTESIAN_POINT('Ctrl Pts',(2.53566592835903,0.600909021307248,-65.3355356979218));
#33965=CARTESIAN_POINT('Ctrl Pts',(2.78735887217201,1.07263972227482,-65.6131842731172));
#33966=CARTESIAN_POINT('Ctrl Pts',(2.83333333333334,1.33275179473161,-65.6666666666667));
#33967=CARTESIAN_POINT('Ctrl Pts',(2.83333333333334,1.5,-65.6666666666667));
#33968=CARTESIAN_POINT('Ctrl Pts',(1.10367510160595,0.00185294611160967,
-64.3391048451961));
#33969=CARTESIAN_POINT('Ctrl Pts',(1.35716302579494,0.0145994266687722,
-64.5939510924519));
#33970=CARTESIAN_POINT('Ctrl Pts',(1.86255136394957,0.173220581778978,-65.0913513637857));
#33971=CARTESIAN_POINT('Ctrl Pts',(2.33553569792179,0.600909021307247,-65.535665928359));
#33972=CARTESIAN_POINT('Ctrl Pts',(2.61318427311724,1.07263972227482,-65.787358872172));
#33973=CARTESIAN_POINT('Ctrl Pts',(2.66666666666667,1.33275179473161,-65.8333333333333));
#33974=CARTESIAN_POINT('Ctrl Pts',(2.66666666666667,1.5,-65.8333333333333));
#33975=CARTESIAN_POINT('Ctrl Pts',(0.868245358015795,0.00185294611160958,
-64.5745345887862));
#33976=CARTESIAN_POINT('Ctrl Pts',(1.12037495913795,0.0145994266687717,
-64.8307391591089));
#33977=CARTESIAN_POINT('Ctrl Pts',(1.63375136411347,0.173220581778977,-65.3201513636217));
#33978=CARTESIAN_POINT('Ctrl Pts',(2.13540546748456,0.600909021307247,-65.7357961587963));
#33979=CARTESIAN_POINT('Ctrl Pts',(2.43900967406247,1.07263972227481,-65.9615334712268));
#33980=CARTESIAN_POINT('Ctrl Pts',(2.5,1.33275179473161,-66.));
#33981=CARTESIAN_POINT('Ctrl Pts',(2.5,1.5,-66.));
#33982=CARTESIAN_POINT('',(3.,1.5,-65.5));
#33983=CARTESIAN_POINT('',(2.5,1.5,-66.));
#33984=CARTESIAN_POINT('Ctrl Pts',(3.,1.5,-65.5));
#33985=CARTESIAN_POINT('Ctrl Pts',(3.,1.33275179473161,-65.5));
#33986=CARTESIAN_POINT('Ctrl Pts',(2.96153347122678,1.07263972227482,-65.4390096740624));
#33987=CARTESIAN_POINT('Ctrl Pts',(2.73579615879626,0.600909021307247,-65.1354054674845));
#33988=CARTESIAN_POINT('Ctrl Pts',(2.32015136362177,0.173220581778977,-64.6337513641135));
#33989=CARTESIAN_POINT('Ctrl Pts',(1.83073915910892,0.0145994266687731,
-64.1203749591379));
#33990=CARTESIAN_POINT('Ctrl Pts',(1.57453458878627,0.00185294611160985,
-63.8682453580158));
#33991=CARTESIAN_POINT('Origin',(2.75,4.,-65.75));
#33992=CARTESIAN_POINT('',(3.,4.,-65.5));
#33993=CARTESIAN_POINT('',(14.375,4.,-54.1249999999998));
#33994=CARTESIAN_POINT('',(3.,4.,-65.5));
#33995=CARTESIAN_POINT('Origin',(1.5,1.5,-41.25));
#33996=CARTESIAN_POINT('',(3.,1.5,-46.9041575982343));
#33997=CARTESIAN_POINT('',(3.,1.5,-41.25));
#33998=CARTESIAN_POINT('Ctrl Pts',(3.,1.5,-46.9041575982343));
#33999=CARTESIAN_POINT('Ctrl Pts',(3.,1.35551296703019,-46.9041575982343));
#34000=CARTESIAN_POINT('Ctrl Pts',(2.97913882256008,1.2141617946757,-46.8845984232444));
#34001=CARTESIAN_POINT('Ctrl Pts',(2.89577102625226,0.928389940435113,-46.8062984441602));
#34002=CARTESIAN_POINT('Ctrl Pts',(2.82982150540341,0.791053413169228,-46.7443046032146));
#34003=CARTESIAN_POINT('Ctrl Pts',(2.64514766490965,0.512937531198892,-46.5701910337406));
#34004=CARTESIAN_POINT('Ctrl Pts',(2.51762496582942,0.38503558873678,-46.4496283712152));
#34005=CARTESIAN_POINT('Ctrl Pts',(2.24921701551044,0.190439066398323,-46.1946602843644));
#34006=CARTESIAN_POINT('Ctrl Pts',(2.10792859962105,0.120380195566533,-46.059925664155));
#34007=CARTESIAN_POINT('Ctrl Pts',(1.81376170731678,0.024706643928065,-45.7780704433202));
#34008=CARTESIAN_POINT('Ctrl Pts',(1.65894854459693,0.000552890155855622,
-45.6290430115594));
#34009=CARTESIAN_POINT('Ctrl Pts',(1.50353740181663,3.12821524572435E-6,
-45.4786905515984));
#34010=CARTESIAN_POINT('Ctrl Pts',(1.50176867612926,1.08300178020774E-19,
-45.4769793019272));
#34011=CARTESIAN_POINT('Ctrl Pts',(1.50000000000001,0.,-45.4752680036083));
#34012=CARTESIAN_POINT('Origin',(3.,4.,-66.));
#34013=CARTESIAN_POINT('',(3.,4.,-46.9041575982343));
#34014=CARTESIAN_POINT('',(3.,4.,-41.25));
#34015=CARTESIAN_POINT('',(3.,4.,-46.9041575982343));
#34016=CARTESIAN_POINT('Origin',(-30.5,0.25,-55.));
#34017=CARTESIAN_POINT('',(-35.55,0.5,-55.));
#34018=CARTESIAN_POINT('',(-35.8,0.25,-55.));
#34019=CARTESIAN_POINT('Origin',(-30.5,0.5,-55.));
#34020=CARTESIAN_POINT('Origin',(-30.5,18.,-55.));
#34021=CARTESIAN_POINT('',(-35.55,17.5,-55.));
#34022=CARTESIAN_POINT('Origin',(-30.5,17.5,-55.));
#34023=CARTESIAN_POINT('',(-35.55,18.,-55.));
#34024=CARTESIAN_POINT('Origin',(30.5,0.25,-55.));
#34025=CARTESIAN_POINT('',(25.45,0.5,-55.));
#34026=CARTESIAN_POINT('',(25.2,0.25,-55.));
#34027=CARTESIAN_POINT('Origin',(30.5,0.5,-55.));
#34028=CARTESIAN_POINT('Origin',(30.5,18.,-55.));
#34029=CARTESIAN_POINT('',(25.45,17.5,-55.));
#34030=CARTESIAN_POINT('Origin',(30.5,17.5,-55.));
#34031=CARTESIAN_POINT('',(25.45,18.,-55.));
#34032=CARTESIAN_POINT('Origin',(35.5422371315094,-2.7,20.6547211791723));
#34033=CARTESIAN_POINT('',(35.7247978384185,0.551098954346127,20.682775911471));
#34034=CARTESIAN_POINT('',(35.3596764246032,1.5,20.6266664468687));
#34035=CARTESIAN_POINT('Ctrl Pts',(35.3596764246032,1.5,20.6266664468687));
#34036=CARTESIAN_POINT('Ctrl Pts',(35.3596764246032,1.31962574714054,20.6266664468687));
#34037=CARTESIAN_POINT('Ctrl Pts',(35.40452588567,1.10798634108372,20.6335586179471));
#34038=CARTESIAN_POINT('Ctrl Pts',(35.5338848608011,0.809115390967544,20.6534376569795));
#34039=CARTESIAN_POINT('Ctrl Pts',(35.6230425085747,0.667215858409758,20.667138819642));
#34040=CARTESIAN_POINT('Ctrl Pts',(35.7247978384207,0.551098954350102,20.6827759114767));
#34041=CARTESIAN_POINT('',(35.3596764208672,-0.844289827423071,20.6266664336486));
#34042=CARTESIAN_POINT('',(35.3596764246032,-2.7,20.6266664468687));
#34043=CARTESIAN_POINT('',(35.7247978384157,-1.8,20.6827759114759));
#34044=CARTESIAN_POINT('Ctrl Pts',(35.7247978384157,-1.8,20.6827759114759));
#34045=CARTESIAN_POINT('Ctrl Pts',(35.7247978384157,-1.61916866909503,20.6827759114759));
#34046=CARTESIAN_POINT('Ctrl Pts',(35.6808305167185,-1.40677945093785,20.6760193017913));
#34047=CARTESIAN_POINT('Ctrl Pts',(35.552259697619,-1.10534194031554,20.6562613814095));
#34048=CARTESIAN_POINT('Ctrl Pts',(35.4623482875555,-0.961189978401695,
20.642444385501));
#34049=CARTESIAN_POINT('Ctrl Pts',(35.3596764103059,-0.84428983506834,20.6266664446716));
#34050=CARTESIAN_POINT('',(35.7247978384157,-2.7,20.6827759114759));
#34051=CARTESIAN_POINT('Origin',(30.5,18.,22.));
#34052=CARTESIAN_POINT('',(25.45,17.5,22.));
#34053=CARTESIAN_POINT('Origin',(30.5,17.5,22.));
#34054=CARTESIAN_POINT('',(25.45,-0.3,22.));
#34055=CARTESIAN_POINT('',(25.45,18.,22.));
#34056=CARTESIAN_POINT('',(34.7765679801409,-0.3,19.3142103002592));
#34057=CARTESIAN_POINT('Origin',(30.5,-0.3,22.));
#34058=CARTESIAN_POINT('Ctrl Pts',(34.7765679801409,-0.3,19.3142103002592));
#34059=CARTESIAN_POINT('Ctrl Pts',(34.9059508242202,-0.300000000000001,
19.5202258822768));
#34060=CARTESIAN_POINT('Ctrl Pts',(35.0195507283414,-0.34517160022148,19.7352882545191));
#34061=CARTESIAN_POINT('Ctrl Pts',(35.2238731819906,-0.522391523218817,
20.1939695646418));
#34062=CARTESIAN_POINT('Ctrl Pts',(35.3033062350033,-0.666213665915556,
20.42817906326));
#34063=CARTESIAN_POINT('Ctrl Pts',(35.3584694985011,-0.840438680575254,
20.6224009726343));
#34064=CARTESIAN_POINT('Ctrl Pts',(35.3590743849931,-0.842362231347438,
20.6245360702757));
#34065=CARTESIAN_POINT('Ctrl Pts',(35.3596764192561,-0.84428983422674,20.6266664279477));
#34066=CARTESIAN_POINT('',(30.7302400397221,1.5,27.0447487077266));
#34067=CARTESIAN_POINT('Origin',(30.5,1.5,22.));
#34068=CARTESIAN_POINT('',(30.7302400397217,-0.844289851346252,27.0447487077266));
#34069=CARTESIAN_POINT('',(30.7302400397221,-2.7,27.0447487077266));
#34070=CARTESIAN_POINT('',(29.3008405049219,-0.3,26.9055597545401));
#34071=CARTESIAN_POINT('Ctrl Pts',(30.7302400397215,-0.84428985134645,27.0447487077266));
#34072=CARTESIAN_POINT('Ctrl Pts',(30.7124846491452,-0.828813695351024,
27.0455590556881));
#34073=CARTESIAN_POINT('Ctrl Pts',(30.6944584562156,-0.813666012125142,
27.0462877270776));
#34074=CARTESIAN_POINT('Ctrl Pts',(30.4892675361419,-0.647229741839043,
27.0534512698364));
#34075=CARTESIAN_POINT('Ctrl Pts',(30.2640772634479,-0.51948243683466,27.0505384638851));
#34076=CARTESIAN_POINT('Ctrl Pts',(29.7858333404989,-0.346841431540347,
27.0046852545821));
#34077=CARTESIAN_POINT('Ctrl Pts',(29.5415138144396,-0.3,26.9643921200114));
#34078=CARTESIAN_POINT('Ctrl Pts',(29.3008405049219,-0.3,26.9055597545401));
#34079=CARTESIAN_POINT('Origin',(30.5,-0.3,22.));
#34080=CARTESIAN_POINT('Origin',(-35.5422371315094,-2.7,20.6547211791723));
#34081=CARTESIAN_POINT('',(-35.7247978384157,-1.8,20.6827759114759));
#34082=CARTESIAN_POINT('',(-35.3596764246031,-0.844289851346258,20.6266664468684));
#34083=CARTESIAN_POINT('Ctrl Pts',(-35.3596764246028,-0.844289851346478,
20.6266664468687));
#34084=CARTESIAN_POINT('Ctrl Pts',(-35.4623482961748,-0.961189991573225,
20.6424443868256));
#34085=CARTESIAN_POINT('Ctrl Pts',(-35.5522597002982,-1.105341946597,20.6562613818212));
#34086=CARTESIAN_POINT('Ctrl Pts',(-35.6808305167185,-1.40677945093785,
20.6760193017913));
#34087=CARTESIAN_POINT('Ctrl Pts',(-35.7247978384157,-1.61916866909503,
20.6827759114759));
#34088=CARTESIAN_POINT('Ctrl Pts',(-35.7247978384157,-1.8,20.6827759114759));
#34089=CARTESIAN_POINT('',(-35.3596764246032,1.5,20.6266664468687));
#34090=CARTESIAN_POINT('',(-35.3596764246032,-2.7,20.6266664468687));
#34091=CARTESIAN_POINT('',(-35.724797838416,0.551098954354631,20.6827759114753));
#34092=CARTESIAN_POINT('Ctrl Pts',(-35.7247978384164,0.55109895435502,20.682775911476));
#34093=CARTESIAN_POINT('Ctrl Pts',(-35.6230425085721,0.667215858413704,
20.6671388196416));
#34094=CARTESIAN_POINT('Ctrl Pts',(-35.5338848608002,0.809115390969431,
20.6534376569794));
#34095=CARTESIAN_POINT('Ctrl Pts',(-35.40452588567,1.10798634108372,20.6335586179471));
#34096=CARTESIAN_POINT('Ctrl Pts',(-35.3596764246032,1.31962574714054,20.6266664468687));
#34097=CARTESIAN_POINT('Ctrl Pts',(-35.3596764246032,1.5,20.6266664468687));
#34098=CARTESIAN_POINT('',(-35.7247978384157,-2.7,20.6827759114759));
#34099=CARTESIAN_POINT('Origin',(-30.5,18.,22.));
#34100=CARTESIAN_POINT('',(-35.55,17.5,22.));
#34101=CARTESIAN_POINT('Origin',(-30.5,17.5,22.));
#34102=CARTESIAN_POINT('',(-35.55,1.5,22.));
#34103=CARTESIAN_POINT('',(-35.55,18.,22.));
#34104=CARTESIAN_POINT('Origin',(-30.5,1.5,22.));
#34105=CARTESIAN_POINT('',(-34.7765679801409,-0.3,19.3142103002592));
#34106=CARTESIAN_POINT('Ctrl Pts',(-35.359676424603,-0.844289851346454,
20.6266664468682));
#34107=CARTESIAN_POINT('Ctrl Pts',(-35.3548608196211,-0.828871170093358,
20.609625952993));
#34108=CARTESIAN_POINT('Ctrl Pts',(-35.3498834808043,-0.813778557683737,
20.5923560119679));
#34109=CARTESIAN_POINT('Ctrl Pts',(-35.291962158532,-0.647352440369088,
20.3954487204406));
#34110=CARTESIAN_POINT('Ctrl Pts',(-35.2181442235994,-0.519566075661792,
20.1826589576689));
#34111=CARTESIAN_POINT('Ctrl Pts',(-35.0237121665274,-0.346861287281918,
19.7432418804637));
#34112=CARTESIAN_POINT('Ctrl Pts',(-34.9083644556171,-0.300000000000001,
19.5240690941071));
#34113=CARTESIAN_POINT('Ctrl Pts',(-34.7765679801409,-0.3,19.3142103002592));
#34114=CARTESIAN_POINT('',(-29.3008405049219,-0.3,26.9055597545401));
#34115=CARTESIAN_POINT('Origin',(-30.5,-0.3,22.));
#34116=CARTESIAN_POINT('',(-30.7302400262003,-0.844289827774839,27.0447487083437));
#34117=CARTESIAN_POINT('Ctrl Pts',(-29.3008405049219,-0.3,26.9055597545401));
#34118=CARTESIAN_POINT('Ctrl Pts',(-29.5371794327976,-0.3,26.9633325844718));
#34119=CARTESIAN_POINT('Ctrl Pts',(-29.7771237213194,-0.34518030422705,
27.0032706405318));
#34120=CARTESIAN_POINT('Ctrl Pts',(-30.2768601749874,-0.522423095905239,
27.0524182450713));
#34121=CARTESIAN_POINT('Ctrl Pts',(-30.52416303416,-0.666251438728489,27.0538881066326));
#34122=CARTESIAN_POINT('Ctrl Pts',(-30.7258446252404,-0.840467297370239,
27.0449478768001));
#34123=CARTESIAN_POINT('Ctrl Pts',(-30.7280449816332,-0.842376569836416,
27.0448488891723));
#34124=CARTESIAN_POINT('Ctrl Pts',(-30.7302400203693,-0.844289834478454,
27.0447487086098));
#34125=CARTESIAN_POINT('',(-30.7302400397221,1.5,27.0447487077266));
#34126=CARTESIAN_POINT('',(-30.7302400397221,-2.7,27.0447487077266));
#34127=CARTESIAN_POINT('Origin',(-30.5,1.5,22.));
#34128=CARTESIAN_POINT('Origin',(-30.8144664255862,-2.7,27.2091305669295));
#34129=CARTESIAN_POINT('',(-30.8986928114466,0.551098954346123,27.3735124261366));
#34130=CARTESIAN_POINT('Ctrl Pts',(-30.7302400397221,1.5,27.0447487077266));
#34131=CARTESIAN_POINT('Ctrl Pts',(-30.7302400397221,1.31962574714054,27.0447487077266));
#34132=CARTESIAN_POINT('Ctrl Pts',(-30.7509318308399,1.10798634108372,27.0851321939616));
#34133=CARTESIAN_POINT('Ctrl Pts',(-30.8106130138229,0.809115390967542,
27.2016099902902));
#34134=CARTESIAN_POINT('Ctrl Pts',(-30.8517468731915,0.667215858409751,
27.2818895868779));
#34135=CARTESIAN_POINT('Ctrl Pts',(-30.8986928114527,0.551098954350096,
27.3735124261369));
#34136=CARTESIAN_POINT('',(-30.8986928114504,-1.8,27.3735124261324));
#34137=CARTESIAN_POINT('Ctrl Pts',(-30.8986928114504,-1.8,27.3735124261324));
#34138=CARTESIAN_POINT('Ctrl Pts',(-30.8986928114504,-1.61916866909503,
27.3735124261324));
#34139=CARTESIAN_POINT('Ctrl Pts',(-30.8784080050129,-1.40677945093785,
27.333923238474));
#34140=CARTESIAN_POINT('Ctrl Pts',(-30.8190904464838,-1.10534194040792,
27.2181551159985));
#34141=CARTESIAN_POINT('Ctrl Pts',(-30.77760883065,-0.961189978595379,27.1371968145879));
#34142=CARTESIAN_POINT('Ctrl Pts',(-30.7302400332229,-0.844289835307704,
27.0447486950422));
#34143=CARTESIAN_POINT('',(-30.8986928114504,-2.7,27.3735124261324));
#34144=CARTESIAN_POINT('Origin',(30.8144664255862,-2.7,27.2091305669295));
#34145=CARTESIAN_POINT('',(30.8986928114504,-1.8,27.3735124261324));
#34146=CARTESIAN_POINT('Ctrl Pts',(30.7302400397219,-0.84428985134648,27.0447487077262));
#34147=CARTESIAN_POINT('Ctrl Pts',(30.7776088345681,-0.961189991573226,
27.1371968222349));
#34148=CARTESIAN_POINT('Ctrl Pts',(30.8190904477017,-1.105341946597,27.2181551183754));
#34149=CARTESIAN_POINT('Ctrl Pts',(30.8784080050129,-1.40677945093785,27.333923238474));
#34150=CARTESIAN_POINT('Ctrl Pts',(30.8986928114504,-1.61916866909503,27.3735124261324));
#34151=CARTESIAN_POINT('Ctrl Pts',(30.8986928114504,-1.8,27.3735124261324));
#34152=CARTESIAN_POINT('',(30.8986928114499,0.551098954354628,27.3735124261329));
#34153=CARTESIAN_POINT('Ctrl Pts',(30.8986928114507,0.551098954355018,27.373512426133));
#34154=CARTESIAN_POINT('Ctrl Pts',(30.8517468731903,0.667215858413702,27.2818895868756));
#34155=CARTESIAN_POINT('Ctrl Pts',(30.8106130138225,0.809115390969429,27.2016099902895));
#34156=CARTESIAN_POINT('Ctrl Pts',(30.7509318308399,1.10798634108372,27.0851321939616));
#34157=CARTESIAN_POINT('Ctrl Pts',(30.7302400397221,1.31962574714054,27.0447487077266));
#34158=CARTESIAN_POINT('Ctrl Pts',(30.7302400397221,1.5,27.0447487077266));
#34159=CARTESIAN_POINT('',(30.8986928114504,-2.7,27.3735124261324));
#34160=CARTESIAN_POINT('Origin',(30.5,17.75,-55.));
#34161=CARTESIAN_POINT('',(24.95,18.,-55.));
#34162=CARTESIAN_POINT('Origin',(30.5,18.,-55.));
#34163=CARTESIAN_POINT('',(25.2,17.75,-55.));
#34164=CARTESIAN_POINT('Origin',(0.,18.,-16.5));
#34165=CARTESIAN_POINT('',(38.,18.,-75.));
#34166=CARTESIAN_POINT('',(64.5,18.,-48.5));
#34167=CARTESIAN_POINT('Origin',(38.,18.,-48.5));
#34168=CARTESIAN_POINT('',(-38.,18.,-75.));
#34169=CARTESIAN_POINT('',(19.,18.,-75.));
#34170=CARTESIAN_POINT('',(-64.5,18.,-48.5));
#34171=CARTESIAN_POINT('Origin',(-38.,18.,-48.5));
#34172=CARTESIAN_POINT('',(-64.5,18.,15.5));
#34173=CARTESIAN_POINT('',(-64.5,18.,-32.5));
#34174=CARTESIAN_POINT('',(-38.,18.,42.));
#34175=CARTESIAN_POINT('Origin',(-38.,18.,15.5));
#34176=CARTESIAN_POINT('',(38.,18.,42.));
#34177=CARTESIAN_POINT('',(-19.,18.,42.));
#34178=CARTESIAN_POINT('',(64.5,18.,15.5));
#34179=CARTESIAN_POINT('Origin',(38.,18.,15.5));
#34180=CARTESIAN_POINT('',(64.5,18.,-0.500000000000003));
#34181=CARTESIAN_POINT('',(-36.05,18.,22.));
#34182=CARTESIAN_POINT('Origin',(-30.5,18.,22.));
#34183=CARTESIAN_POINT('',(-36.05,18.,-55.));
#34184=CARTESIAN_POINT('Origin',(-30.5,18.,-55.));
#34185=CARTESIAN_POINT('',(-59.2,18.,7.34788079488411E-16));
#34186=CARTESIAN_POINT('Origin',(-53.2,18.,0.));
#34187=CARTESIAN_POINT('',(26.05,18.,4.44089209850063E-15));
#34188=CARTESIAN_POINT('',(26.05,18.,-33.));
#34189=CARTESIAN_POINT('',(26.05,18.,-24.75));
#34190=CARTESIAN_POINT('',(-26.05,18.,0.));
#34191=CARTESIAN_POINT('Origin',(0.,18.,0.));
#34192=CARTESIAN_POINT('',(-26.05,18.,-33.));
#34193=CARTESIAN_POINT('',(-26.05,18.,-8.25));
#34194=CARTESIAN_POINT('Origin',(0.,18.,-33.));
#34195=CARTESIAN_POINT('',(26.49,18.,-16.5));
#34196=CARTESIAN_POINT('Origin',(30.5,18.,-16.5));
#34197=CARTESIAN_POINT('',(-34.51,18.,-16.5));
#34198=CARTESIAN_POINT('Origin',(-30.5,18.,-16.5));
#34199=CARTESIAN_POINT('',(47.2,18.,7.34788079488411E-16));
#34200=CARTESIAN_POINT('Origin',(53.2,18.,0.));
#34201=CARTESIAN_POINT('',(24.95,18.,22.));
#34202=CARTESIAN_POINT('Origin',(30.5,18.,22.));
#34203=CARTESIAN_POINT('Origin',(-30.5,17.75,22.));
#34204=CARTESIAN_POINT('',(-35.8,17.75,22.));
#34205=CARTESIAN_POINT('Origin',(30.5,17.75,22.));
#34206=CARTESIAN_POINT('',(25.2,17.75,22.));
#34207=CARTESIAN_POINT('Origin',(-30.5,17.75,-55.));
#34208=CARTESIAN_POINT('',(-35.8,17.75,-55.));
#34209=CARTESIAN_POINT('Origin',(53.2,17.75,0.));
#34210=CARTESIAN_POINT('',(47.7,17.5,-6.73555739531044E-16));
#34211=CARTESIAN_POINT('',(47.45,17.75,7.04171909509728E-16));
#34212=CARTESIAN_POINT('Origin',(53.2,17.5,0.));
#34213=CARTESIAN_POINT('Origin',(53.2,-0.1,0.));
#34214=CARTESIAN_POINT('',(47.7,0.5,6.73555739531044E-16));
#34215=CARTESIAN_POINT('Origin',(53.2,0.5,0.));
#34216=CARTESIAN_POINT('',(47.7,-0.1,6.73555739531044E-16));
#34217=CARTESIAN_POINT('Origin',(-53.2,17.75,0.));
#34218=CARTESIAN_POINT('',(-58.7,17.5,-6.73555739531044E-16));
#34219=CARTESIAN_POINT('',(-58.95,17.75,7.04171909509728E-16));
#34220=CARTESIAN_POINT('Origin',(-53.2,17.5,0.));
#34221=CARTESIAN_POINT('Origin',(-53.2,-0.1,0.));
#34222=CARTESIAN_POINT('',(-58.7,0.5,6.73555739531044E-16));
#34223=CARTESIAN_POINT('Origin',(-53.2,0.5,0.));
#34224=CARTESIAN_POINT('',(-58.7,-0.1,6.73555739531044E-16));
#34225=CARTESIAN_POINT('Ctrl Pts',(-46.2750334800828,0.00185294611160958,
-44.0483053101957));
#34226=CARTESIAN_POINT('Ctrl Pts',(-46.2692140102843,0.00164657951619625,
-44.0483519609257));
#34227=CARTESIAN_POINT('Ctrl Pts',(-46.2265311890134,0.000220053554164141,
-44.0487734988259));
#34228=CARTESIAN_POINT('Ctrl Pts',(-46.1797598454879,1.29647441628285E-5,
-44.0493466615837));
#34229=CARTESIAN_POINT('Ctrl Pts',(-46.1722185099715,-1.25208261182028E-17,
-44.0494259364697));
#34230=CARTESIAN_POINT('Ctrl Pts',(-46.1707625875413,0.,-44.0494422439817));
#34231=CARTESIAN_POINT('Ctrl Pts',(-46.2750334800828,0.00185294611160958,
-44.3812532465669));
#34232=CARTESIAN_POINT('Ctrl Pts',(-46.2692140102843,0.0016465795161962,
-44.3812687968102));
#34233=CARTESIAN_POINT('Ctrl Pts',(-46.2265311890134,0.000220053554164124,
-44.3813630297282));
#34234=CARTESIAN_POINT('Ctrl Pts',(-46.1797598454879,1.29647441628394E-5,
-44.3816138834835));
#34235=CARTESIAN_POINT('Ctrl Pts',(-46.1722185099715,-7.54565250469149E-18,
-44.3816267886582));
#34236=CARTESIAN_POINT('Ctrl Pts',(-46.1707625875413,0.,-44.3816322244955));
#34237=CARTESIAN_POINT('Ctrl Pts',(-46.2750334800828,0.00185294611160958,
-44.7142011829381));
#34238=CARTESIAN_POINT('Ctrl Pts',(-46.2692140102843,0.00164657951619616,
-44.7141856326948));
#34239=CARTESIAN_POINT('Ctrl Pts',(-46.2264061493503,-2.42006109810558E-5,
-44.7139663601137));
#34240=CARTESIAN_POINT('Ctrl Pts',(-46.1797424783604,0.000164604021204162,
-44.7138231788941));
#34241=CARTESIAN_POINT('Ctrl Pts',(-46.1722185099715,-2.56641760752889E-18,
-44.7138276408467));
#34242=CARTESIAN_POINT('Ctrl Pts',(-46.1707625875413,0.,-44.7138222050094));
#34243=CARTESIAN_POINT('Ctrl Pts',(-46.2750334800828,0.00185294611160958,
-45.0471491193093));
#34244=CARTESIAN_POINT('Ctrl Pts',(-46.2692140102843,0.00164657951619612,
-45.0471024685793));
#34245=CARTESIAN_POINT('Ctrl Pts',(-46.2265311890134,0.000220053554162325,
-45.0466809306791));
#34246=CARTESIAN_POINT('Ctrl Pts',(-46.1797598454878,1.29647441628376E-5,
-45.0461077679213));
#34247=CARTESIAN_POINT('Ctrl Pts',(-46.1722185099715,2.40785117657972E-18,
-45.0460284930352));
#34248=CARTESIAN_POINT('Ctrl Pts',(-46.1707625875413,0.,-45.0460121855233));
#34249=CARTESIAN_POINT('',(-46.2750334800828,0.00185294611160958,-44.0483053101957));
#34250=CARTESIAN_POINT('Ctrl Pts',(-46.1707625875413,-2.22044604925031E-16,
-44.0494422439817));
#34251=CARTESIAN_POINT('Ctrl Pts',(-46.1712260120785,-2.29034413256906E-16,
-44.0494370532511));
#34252=CARTESIAN_POINT('Ctrl Pts',(-46.1716940067242,9.12216844862265E-8,
-44.0494318096041));
#34253=CARTESIAN_POINT('Ctrl Pts',(-46.1722703781186,3.87472611551587E-7,
-44.0494252934764));
#34254=CARTESIAN_POINT('Ctrl Pts',(-46.1728752899714,6.98393137625681E-7,
-44.0494184546864));
#34255=CARTESIAN_POINT('Ctrl Pts',(-46.1735992866602,1.23194503986655E-6,
-44.0494102174312));
#34256=CARTESIAN_POINT('Ctrl Pts',(-46.1745042934384,2.38657547613208E-6,
-44.0493998460925));
#34257=CARTESIAN_POINT('Ctrl Pts',(-46.1754684855519,3.61671605358732E-6,
-44.0493887964925));
#34258=CARTESIAN_POINT('Ctrl Pts',(-46.1766377387174,5.55516755122873E-6,
-44.0493753288015));
#34259=CARTESIAN_POINT('Ctrl Pts',(-46.1780277790772,8.99934440856676E-6,
-44.0493592449597));
#34260=CARTESIAN_POINT('Ctrl Pts',(-46.1795622676003,1.28014281552638E-5,
-44.0493414897409));
#34261=CARTESIAN_POINT('Ctrl Pts',(-46.1813652342406,1.84658046869166E-5,
-44.0493205524466));
#34262=CARTESIAN_POINT('Ctrl Pts',(-46.183395156043,2.72127176232928E-5,
-44.0492969087164));
#34263=CARTESIAN_POINT('Ctrl Pts',(-46.1859419093286,3.81866523005328E-5,
-44.0492672451365));
#34264=CARTESIAN_POINT('Ctrl Pts',(-46.1888446371058,5.41281456188157E-5,
-44.049233333982));
#34265=CARTESIAN_POINT('Ctrl Pts',(-46.1919381576189,7.64762491831661E-5,
-44.0491971278456));
#34266=CARTESIAN_POINT('Ctrl Pts',(-46.1952200088624,0.000100184885075284,
-44.0491587175124));
#34267=CARTESIAN_POINT('Ctrl Pts',(-46.198709812785,0.000131146817816346,
-44.0491178019999));
#34268=CARTESIAN_POINT('Ctrl Pts',(-46.2021957015517,0.000168532538723509,
-44.0490769551091));
#34269=CARTESIAN_POINT('Ctrl Pts',(-46.2048367108624,0.000196857033166613,
-44.0490460083331));
#34270=CARTESIAN_POINT('Ctrl Pts',(-46.207474324971,0.000228767928640852,
-44.0490151153336));
#34271=CARTESIAN_POINT('Ctrl Pts',(-46.2100500271557,0.000263295917068085,
-44.0489850380078));
#34272=CARTESIAN_POINT('Ctrl Pts',(-46.2123742451676,0.000294452691750434,
-44.0489578973459));
#34273=CARTESIAN_POINT('Ctrl Pts',(-46.2146474763278,0.000327690884695818,
-44.0489314272062));
#34274=CARTESIAN_POINT('Ctrl Pts',(-46.2168680460012,0.000362622665149637,
-44.0489057363541));
#34275=CARTESIAN_POINT('Ctrl Pts',(-46.2190586240439,0.000397082647276686,
-44.0488803924898));
#34276=CARTESIAN_POINT('Ctrl Pts',(-46.2211970152928,0.000433137034800887,
-44.0488558169149));
#34277=CARTESIAN_POINT('Ctrl Pts',(-46.2233355230111,0.00047149090490195,
-44.0488315276206));
#34278=CARTESIAN_POINT('Ctrl Pts',(-46.2254211663469,0.000508896658874311,
-44.048807838763));
#34279=CARTESIAN_POINT('Ctrl Pts',(-46.2275162736585,0.000548663598881684,
-44.048784324577));
#34280=CARTESIAN_POINT('Ctrl Pts',(-46.229662604295,0.000591779397137282,
-44.0487605858922));
#34281=CARTESIAN_POINT('Ctrl Pts',(-46.2319694831195,0.000638120310465147,
-44.0487350715244));
#34282=CARTESIAN_POINT('Ctrl Pts',(-46.2343350335908,0.000688360290181702,
-44.0487093036337));
#34283=CARTESIAN_POINT('Ctrl Pts',(-46.2367509866092,0.000742716673596044,
-44.0486833825405));
#34284=CARTESIAN_POINT('Ctrl Pts',(-46.2395110312765,0.000804814754574078,
-44.0486537696405));
#34285=CARTESIAN_POINT('Ctrl Pts',(-46.2423361082531,0.000872336312489005,
-44.0486239662077));
#34286=CARTESIAN_POINT('Ctrl Pts',(-46.2451470433618,0.000943604228376804,
-44.0485947611566));
#34287=CARTESIAN_POINT('Ctrl Pts',(-46.2490414567667,0.00104234244759405,
-44.0485542989836));
#34288=CARTESIAN_POINT('Ctrl Pts',(-46.2529045939084,0.00114840209597425,
-44.0485150363574));
#34289=CARTESIAN_POINT('Ctrl Pts',(-46.2564328497428,0.00125139174850086,
-44.0484798418561));
#34290=CARTESIAN_POINT('Ctrl Pts',(-46.2590790416185,0.00132863398789582,
-44.0484534459802));
#34291=CARTESIAN_POINT('Ctrl Pts',(-46.261533087147,0.00140389724199395,
-44.0484293702208));
#34292=CARTESIAN_POINT('Ctrl Pts',(-46.2636886623346,0.00147212889993908,
-44.0484085450809));
#34293=CARTESIAN_POINT('Ctrl Pts',(-46.2654946449701,0.00152929470429269,
-44.0483910973753));
#34294=CARTESIAN_POINT('Ctrl Pts',(-46.267090598365,0.00158146111034102,
-44.0483759344752));
#34295=CARTESIAN_POINT('Ctrl Pts',(-46.2684508145559,0.00162671007904525,
-44.0483632289425));
#34296=CARTESIAN_POINT('Ctrl Pts',(-46.2697296616146,0.00166925222118772,
-44.048351283464));
#34297=CARTESIAN_POINT('Ctrl Pts',(-46.2707995465537,0.00170564250685707,
-44.048341514987));
#34298=CARTESIAN_POINT('Ctrl Pts',(-46.2716824580706,0.0017359725457522,
-44.0483336475365));
#34299=CARTESIAN_POINT('Ctrl Pts',(-46.2725053682963,0.0017642414024576,
-44.0483263147457));
#34300=CARTESIAN_POINT('Ctrl Pts',(-46.273165643982,0.00178723762246348,
-44.0483206352252));
#34301=CARTESIAN_POINT('Ctrl Pts',(-46.2737251009273,0.00180683428706385,
-44.0483159663184));
#34302=CARTESIAN_POINT('Ctrl Pts',(-46.2742130349626,0.00182392564631187,
-44.0483118943007));
#34303=CARTESIAN_POINT('Ctrl Pts',(-46.2746246568584,0.00183844866426981,
-44.0483085874533));
#34304=CARTESIAN_POINT('Ctrl Pts',(-46.2750334800827,0.00185294611160836,
-44.0483053101957));
#34305=CARTESIAN_POINT('',(-46.2750334800828,0.00185294611160958,-45.0471491193093));
#34306=CARTESIAN_POINT('Ctrl Pts',(-46.2750334800828,0.00185294611160958,
-45.0471491193093));
#34307=CARTESIAN_POINT('Ctrl Pts',(-46.2750334800828,0.00185294611160958,
-44.7142011829381));
#34308=CARTESIAN_POINT('Ctrl Pts',(-46.2750334800828,0.00185294611160958,
-44.3812532465669));
#34309=CARTESIAN_POINT('Ctrl Pts',(-46.2750334800828,0.00185294611160958,
-44.0483053101957));
#34310=CARTESIAN_POINT('Ctrl Pts',(-46.2750334800828,0.00185294611160991,
-45.0471491193093));
#34311=CARTESIAN_POINT('Ctrl Pts',(-46.2745703659484,0.00183652343213913,
-45.0471454068384));
#34312=CARTESIAN_POINT('Ctrl Pts',(-46.2741026813164,0.00182002913551302,
-45.0471416470788));
#34313=CARTESIAN_POINT('Ctrl Pts',(-46.2735266846993,0.00179989061882035,
-45.0471368004589));
#34314=CARTESIAN_POINT('Ctrl Pts',(-46.272922163659,0.00177875480534642,
-45.0471317138253));
#34315=CARTESIAN_POINT('Ctrl Pts',(-46.2721986280875,0.00175361200744172,
-45.0471254328191));
#34316=CARTESIAN_POINT('Ctrl Pts',(-46.2712941819279,0.00172265954511253,
-45.0471173077251));
#34317=CARTESIAN_POINT('Ctrl Pts',(-46.2703305802151,0.00168968262836036,
-45.047108651207));
#34318=CARTESIAN_POINT('Ctrl Pts',(-46.2691620271534,0.00165012867729241,
-45.0470979049924));
#34319=CARTESIAN_POINT('Ctrl Pts',(-46.2677727834885,0.00160423233980689,
-45.0470848469776));
#34320=CARTESIAN_POINT('Ctrl Pts',(-46.2662391395715,0.00155356546215624,
-45.0470704316916));
#34321=CARTESIAN_POINT('Ctrl Pts',(-46.2644371217823,0.001495217018528,
-45.0470532033005));
#34322=CARTESIAN_POINT('Ctrl Pts',(-46.2624081930856,0.00143187557828095,
-45.0470334723104));
#34323=CARTESIAN_POINT('Ctrl Pts',(-46.2598623899414,0.00135239775434378,
-45.0470087148033));
#34324=CARTESIAN_POINT('Ctrl Pts',(-46.2569605947754,0.00126521876820982,
-45.0469800244132));
#34325=CARTESIAN_POINT('Ctrl Pts',(-46.2538679066071,0.00117763891592237,
-45.0469488787412));
#34326=CARTESIAN_POINT('Ctrl Pts',(-46.2505882042891,0.00108476312989613,
-45.0469158496975));
#34327=CARTESIAN_POINT('Ctrl Pts',(-46.2471005941737,0.000991719524369893,
-45.0468801237951));
#34328=CARTESIAN_POINT('Ctrl Pts',(-46.2436166498116,0.000905201076382811,
-45.0468437234767));
#34329=CARTESIAN_POINT('Ctrl Pts',(-46.2409766290361,0.0008396401843567,
-45.0468161404883));
#34330=CARTESIAN_POINT('Ctrl Pts',(-46.2383398635848,0.000777766532132296,
-45.0467881851458));
#34331=CARTESIAN_POINT('Ctrl Pts',(-46.2357648305552,0.00072069456144308,
-45.0467604449209));
#34332=CARTESIAN_POINT('Ctrl Pts',(-46.2334411807933,0.00066919414588216,
-45.0467354127887));
#34333=CARTESIAN_POINT('Ctrl Pts',(-46.2311683745646,0.000621574660653182,
-45.0467105626822));
#34334=CARTESIAN_POINT('Ctrl Pts',(-46.2289480715865,0.000577512604324371,
-45.0466859283192));
#34335=CARTESIAN_POINT('Ctrl Pts',(-46.2267571009757,0.000534032650722002,
-45.0466616194001));
#34336=CARTESIAN_POINT('Ctrl Pts',(-46.2246181983236,0.000493996445433125,
-45.0466375306524));
#34337=CARTESIAN_POINT('Ctrl Pts',(-46.2224789858344,0.000456253937658024,
-45.0466131580609));
#34338=CARTESIAN_POINT('Ctrl Pts',(-46.2203933191886,0.000419456148754817,
-45.0465893955308));
#34339=CARTESIAN_POINT('Ctrl Pts',(-46.2182980063535,0.000384680303810759,
-45.0465652657332));
#34340=CARTESIAN_POINT('Ctrl Pts',(-46.2161513192572,0.000351435419324808,
-45.0465403951498));
#34341=CARTESIAN_POINT('Ctrl Pts',(-46.2138440203937,0.000315703204635488,
-45.0465136637883));
#34342=CARTESIAN_POINT('Ctrl Pts',(-46.2114778723633,0.000281787957705771,
-45.0464860818021));
#34343=CARTESIAN_POINT('Ctrl Pts',(-46.2090611791439,0.000250206967382205,
-45.0464578399095));
#34344=CARTESIAN_POINT('Ctrl Pts',(-46.2063001182845,0.000214125831560948,
-45.0464255736774));
#34345=CARTESIAN_POINT('Ctrl Pts',(-46.2034738288062,0.00018116946976453,
-45.046392454497));
#34346=CARTESIAN_POINT('Ctrl Pts',(-46.2006615752144,0.000152480845408531,
-45.0463594963285));
#34347=CARTESIAN_POINT('Ctrl Pts',(-46.1967660663297,0.000112741615848296,
-45.046313842964));
#34348=CARTESIAN_POINT('Ctrl Pts',(-46.1929016183748,8.14691463179917E-5,
-45.0462685501633));
#34349=CARTESIAN_POINT('Ctrl Pts',(-46.1893720134758,5.90616066560301E-5,
-45.0462272825148));
#34350=CARTESIAN_POINT('Ctrl Pts',(-46.1867248098016,4.22559519095589E-5,
-45.0461963317784));
#34351=CARTESIAN_POINT('Ctrl Pts',(-46.1842697342872,3.03183594517789E-5,
-45.0461676865023));
#34352=CARTESIAN_POINT('Ctrl Pts',(-46.1821131987253,2.19691435525693E-5,
-45.0461425976401));
#34353=CARTESIAN_POINT('Ctrl Pts',(-46.1803063686599,1.49738430462828E-5,
-45.0461215772074));
#34354=CARTESIAN_POINT('Ctrl Pts',(-46.1787096280764,1.04521897691233E-5,
-45.0461030584842));
#34355=CARTESIAN_POINT('Ctrl Pts',(-46.1773487225908,7.39546431272053E-6,
-45.0460873323693));
#34356=CARTESIAN_POINT('Ctrl Pts',(-46.1760692107157,4.52155678447191E-6,
-45.0460725468084));
#34357=CARTESIAN_POINT('Ctrl Pts',(-46.1749987537671,2.92603171308054E-6,
-45.0460602361923));
#34358=CARTESIAN_POINT('Ctrl Pts',(-46.1741153616204,1.91616332645417E-6,
-45.0460501300432));
#34359=CARTESIAN_POINT('Ctrl Pts',(-46.1732919932801,9.74912421790196E-7,
-45.0460407105763));
#34360=CARTESIAN_POINT('Ctrl Pts',(-46.1726313429966,5.41797940506856E-7,
-45.0460332083471));
#34361=CARTESIAN_POINT('Ctrl Pts',(-46.172071556338,2.9201856199812E-7,
-45.0460268901009));
#34362=CARTESIAN_POINT('Ctrl Pts',(-46.171583423441,7.42114211156187E-8,
-45.0460213806022));
#34363=CARTESIAN_POINT('Ctrl Pts',(-46.1711716076359,-2.2137356598813E-16,
-45.0460167668801));
#34364=CARTESIAN_POINT('Ctrl Pts',(-46.1707625875413,-2.22044604925031E-16,
-45.0460121855233));
#34365=CARTESIAN_POINT('Ctrl Pts',(-46.2750334800828,0.00185294611160958,
-45.0471491193093));
#34366=CARTESIAN_POINT('Ctrl Pts',(-46.814203289689,0.0209726669473543,
-45.0514712768415));
#34367=CARTESIAN_POINT('Ctrl Pts',(-47.6898108873463,0.308848973617175,
-45.0129318213479));
#34368=CARTESIAN_POINT('Ctrl Pts',(-48.346446182696,0.985587673094209,-44.9222599738363));
#34369=CARTESIAN_POINT('Ctrl Pts',(-48.4368145112785,1.33275179473165,-44.9012806053457));
#34370=CARTESIAN_POINT('Ctrl Pts',(-48.4368145112785,1.50000000000004,-44.9012806053457));
#34371=CARTESIAN_POINT('Ctrl Pts',(-46.2750334800828,0.00185294611160958,
-44.7142011829381));
#34372=CARTESIAN_POINT('Ctrl Pts',(-46.814203289689,0.0209726669473542,
-44.7156419021155));
#34373=CARTESIAN_POINT('Ctrl Pts',(-47.6898108873463,0.308848973617175,
-44.702795416951));
#34374=CARTESIAN_POINT('Ctrl Pts',(-48.346446182696,0.985587673094209,-44.6725714677804));
#34375=CARTESIAN_POINT('Ctrl Pts',(-48.4368145112785,1.33275179473165,-44.6655783449502));
#34376=CARTESIAN_POINT('Ctrl Pts',(-48.4368145112785,1.50000000000004,-44.6655783449502));
#34377=CARTESIAN_POINT('Ctrl Pts',(-46.2750334800828,0.00185294611160958,
-44.3812532465669));
#34378=CARTESIAN_POINT('Ctrl Pts',(-46.814203289689,0.0209726669473541,
-44.3798125273895));
#34379=CARTESIAN_POINT('Ctrl Pts',(-47.6898108873463,0.308848973617173,
-44.392659012554));
#34380=CARTESIAN_POINT('Ctrl Pts',(-48.346446182696,0.985587673094209,-44.4228829617245));
#34381=CARTESIAN_POINT('Ctrl Pts',(-48.4368145112785,1.33275179473165,-44.4298760845547));
#34382=CARTESIAN_POINT('Ctrl Pts',(-48.4368145112785,1.50000000000003,-44.4298760845547));
#34383=CARTESIAN_POINT('Ctrl Pts',(-46.2750334800828,0.00185294611160958,
-44.0483053101957));
#34384=CARTESIAN_POINT('Ctrl Pts',(-46.814203289689,0.020972666947354,-44.0439831526635));
#34385=CARTESIAN_POINT('Ctrl Pts',(-47.6898108873463,0.308848973617173,
-44.0825226081571));
#34386=CARTESIAN_POINT('Ctrl Pts',(-48.346446182696,0.985587673094209,-44.1731944556686));
#34387=CARTESIAN_POINT('Ctrl Pts',(-48.4368145112785,1.33275179473165,-44.1941738241592));
#34388=CARTESIAN_POINT('Ctrl Pts',(-48.4368145112785,1.50000000000003,-44.1941738241592));
#34389=CARTESIAN_POINT('',(-48.4368145112785,1.50000000000002,-44.1941738241592));
#34390=CARTESIAN_POINT('Ctrl Pts',(-46.2750334800828,0.00185294611160958,
-44.0483053101957));
#34391=CARTESIAN_POINT('Ctrl Pts',(-46.814203289689,0.020972666947354,-44.0439831526635));
#34392=CARTESIAN_POINT('Ctrl Pts',(-47.6898108873463,0.308848973617173,
-44.0825226081571));
#34393=CARTESIAN_POINT('Ctrl Pts',(-48.346446182696,0.985587673094209,-44.1731944556686));
#34394=CARTESIAN_POINT('Ctrl Pts',(-48.4368145112785,1.33275179473165,-44.1941738241592));
#34395=CARTESIAN_POINT('Ctrl Pts',(-48.4368145112785,1.50000000000003,-44.1941738241592));
#34396=CARTESIAN_POINT('',(-48.4368145112785,1.50000000000002,-44.9012806053457));
#34397=CARTESIAN_POINT('',(-48.4368145112785,1.50000000000002,-44.1941738241592));
#34398=CARTESIAN_POINT('Ctrl Pts',(-48.4368145112785,1.50000000000004,-44.9012806053457));
#34399=CARTESIAN_POINT('Ctrl Pts',(-48.4368145112785,1.33275179473165,-44.9012806053457));
#34400=CARTESIAN_POINT('Ctrl Pts',(-48.346446182696,0.985587673094209,-44.9222599738363));
#34401=CARTESIAN_POINT('Ctrl Pts',(-47.6898108873463,0.308848973617175,
-45.0129318213479));
#34402=CARTESIAN_POINT('Ctrl Pts',(-46.814203289689,0.0209726669473543,
-45.0514712768415));
#34403=CARTESIAN_POINT('Ctrl Pts',(-46.2750334800828,0.00185294611160958,
-45.0471491193093));
#34404=CARTESIAN_POINT('Origin',(-48.4368145112785,4.,-44.5477272147525));
#34405=CARTESIAN_POINT('',(-48.4368145112785,4.,-44.1941738241592));
#34406=CARTESIAN_POINT('',(-48.4368145112785,4.,-44.9012806053458));
#34407=CARTESIAN_POINT('',(-48.4368145112785,4.,-30.5238636073762));
#34408=CARTESIAN_POINT('',(-48.4368145112785,4.,-44.9012806053458));
#34409=CARTESIAN_POINT('',(-48.4368145112785,4.,-44.1941738241592));
#34410=CARTESIAN_POINT('Origin',(-42.5440475583121,1.5,-48.6727272147525));
#34411=CARTESIAN_POINT('',(-44.9012806053458,1.5,-48.4368145112785));
#34412=CARTESIAN_POINT('',(-43.6047077300919,1.5,-49.7333873865323));
#34413=CARTESIAN_POINT('',(-45.0471491193093,0.00185294611161013,-46.2750334800827));
#34414=CARTESIAN_POINT('Ctrl Pts',(-45.0471491193093,0.00185294611161013,
-46.2750334800827));
#34415=CARTESIAN_POINT('Ctrl Pts',(-45.0514712768415,0.0209726669473565,
-46.8142032896889));
#34416=CARTESIAN_POINT('Ctrl Pts',(-45.0129318213479,0.308848973617163,
-47.6898108873462));
#34417=CARTESIAN_POINT('Ctrl Pts',(-44.9222599738363,0.985587673094179,
-48.3464461826959));
#34418=CARTESIAN_POINT('Ctrl Pts',(-44.9012806053458,1.33275179473162,-48.4368145112785));
#34419=CARTESIAN_POINT('Ctrl Pts',(-44.9012806053458,1.5,-48.4368145112785));
#34420=CARTESIAN_POINT('Ctrl Pts',(-45.0460121855233,-2.22044604925031E-16,
-46.1707625875413));
#34421=CARTESIAN_POINT('Ctrl Pts',(-45.0460173762539,-2.21088104837496E-16,
-46.1712260120786));
#34422=CARTESIAN_POINT('Ctrl Pts',(-45.0460226199009,9.12216842420496E-8,
-46.1716940067243));
#34423=CARTESIAN_POINT('Ctrl Pts',(-45.0460291360286,3.87472611329542E-7,
-46.1722703781187));
#34424=CARTESIAN_POINT('Ctrl Pts',(-45.0460359748186,6.98393137422036E-7,
-46.1728752899715));
#34425=CARTESIAN_POINT('Ctrl Pts',(-45.0460442120738,1.23194503982883E-6,
-46.1735992866603));
#34426=CARTESIAN_POINT('Ctrl Pts',(-45.0460545834124,2.38657547613208E-6,
-46.1745042934385));
#34427=CARTESIAN_POINT('Ctrl Pts',(-45.0460656330125,3.61671605361644E-6,
-46.175468485552));
#34428=CARTESIAN_POINT('Ctrl Pts',(-45.0460791007035,5.55516755121E-6,-46.1766377387174));
#34429=CARTESIAN_POINT('Ctrl Pts',(-45.0460951845453,8.99934440856676E-6,
-46.1780277790772));
#34430=CARTESIAN_POINT('Ctrl Pts',(-45.0461129397641,1.2801428155372E-5,
-46.1795622676004));
#34431=CARTESIAN_POINT('Ctrl Pts',(-45.0461338770584,1.84658046875068E-5,
-46.1813652342407));
#34432=CARTESIAN_POINT('Ctrl Pts',(-45.0461575207886,2.7212717624181E-5,
-46.1833951560432));
#34433=CARTESIAN_POINT('Ctrl Pts',(-45.0461871843685,3.81866523016351E-5,
-46.1859419093288));
#34434=CARTESIAN_POINT('Ctrl Pts',(-45.046221095523,5.41281456200928E-5,
-46.188844637106));
#34435=CARTESIAN_POINT('Ctrl Pts',(-45.0462573016594,7.64762491847204E-5,
-46.1919381576191));
#34436=CARTESIAN_POINT('Ctrl Pts',(-45.0462957119926,0.000100184885075293,
-46.1952200088624));
#34437=CARTESIAN_POINT('Ctrl Pts',(-45.0463366275051,0.000131146817813724,
-46.1987098127846));
#34438=CARTESIAN_POINT('Ctrl Pts',(-45.0463774743959,0.000168532538717292,
-46.2021957015511));
#34439=CARTESIAN_POINT('Ctrl Pts',(-45.0464084211719,0.000196857033159762,
-46.2048367108618));
#34440=CARTESIAN_POINT('Ctrl Pts',(-45.0464393141714,0.000228767928633612,
-46.2074743249703));
#34441=CARTESIAN_POINT('Ctrl Pts',(-45.0464693914972,0.000263295917060313,
-46.210050027155));
#34442=CARTESIAN_POINT('Ctrl Pts',(-45.0464965321591,0.000294452691741994,
-46.2123742451669));
#34443=CARTESIAN_POINT('Ctrl Pts',(-45.0465230022988,0.000327690884686502,
-46.2146474763272));
#34444=CARTESIAN_POINT('Ctrl Pts',(-45.0465486931509,0.000362622665139645,
-46.2168680460005));
#34445=CARTESIAN_POINT('Ctrl Pts',(-45.0465740370152,0.000397082647263859,
-46.2190586240431));
#34446=CARTESIAN_POINT('Ctrl Pts',(-45.0465986125901,0.000433137034784962,
-46.2211970152918));
#34447=CARTESIAN_POINT('Ctrl Pts',(-45.0466229018844,0.00047149090488241,
-46.22333552301));
#34448=CARTESIAN_POINT('Ctrl Pts',(-45.046646590742,0.000508896658854249,
-46.2254211663458));
#34449=CARTESIAN_POINT('Ctrl Pts',(-45.046670104928,0.00054866359886092,
-46.2275162736575));
#34450=CARTESIAN_POINT('Ctrl Pts',(-45.0466938436128,0.000591779397115744,
-46.2296626042939));
#34451=CARTESIAN_POINT('Ctrl Pts',(-45.0467193579806,0.00063812031043945,
-46.2319694831182));
#34452=CARTESIAN_POINT('Ctrl Pts',(-45.0467451258713,0.000688360290151415,
-46.2343350335893));
#34453=CARTESIAN_POINT('Ctrl Pts',(-45.0467710469645,0.000742716673560517,
-46.2367509866076));
#34454=CARTESIAN_POINT('Ctrl Pts',(-45.0468006598645,0.000804814754530438,
-46.2395110312746));
#34455=CARTESIAN_POINT('Ctrl Pts',(-45.0468304632973,0.00087233631243586,
-46.2423361082509));
#34456=CARTESIAN_POINT('Ctrl Pts',(-45.0468596683484,0.000943604228314632,
-46.2451470433594));
#34457=CARTESIAN_POINT('Ctrl Pts',(-45.0469001305214,0.00104234244753431,
-46.2490414567645));
#34458=CARTESIAN_POINT('Ctrl Pts',(-45.0469393931475,0.0011484020959196,
-46.2529045939064));
#34459=CARTESIAN_POINT('Ctrl Pts',(-45.0469745876488,0.0012513917484529,
-46.2564328497411));
#34460=CARTESIAN_POINT('Ctrl Pts',(-45.0470009835248,0.00132863398785288,
-46.2590790416171));
#34461=CARTESIAN_POINT('Ctrl Pts',(-45.0470250592842,0.00140389724195716,
-46.2615330871458));
#34462=CARTESIAN_POINT('Ctrl Pts',(-45.0470458844242,0.00147212889990822,
-46.2636886623335));
#34463=CARTESIAN_POINT('Ctrl Pts',(-45.0470633321297,0.00152929470426462,
-46.2654946449692));
#34464=CARTESIAN_POINT('Ctrl Pts',(-45.0470784950298,0.00158146111031593,
-46.2670905983642));
#34465=CARTESIAN_POINT('Ctrl Pts',(-45.0470912005626,0.00162671007902326,
-46.2684508145552));
#34466=CARTESIAN_POINT('Ctrl Pts',(-45.047103146041,0.00166925222116762,
-46.269729661614));
#34467=CARTESIAN_POINT('Ctrl Pts',(-45.047112914518,0.00170564250683925,
-46.2707995465531));
#34468=CARTESIAN_POINT('Ctrl Pts',(-45.0471207819685,0.00173597254573643,
-46.2716824580701));
#34469=CARTESIAN_POINT('Ctrl Pts',(-45.0471281147594,0.00176424140244397,
-46.2725053682959));
#34470=CARTESIAN_POINT('Ctrl Pts',(-45.0471337942798,0.00178723762245191,
-46.2731656439817));
#34471=CARTESIAN_POINT('Ctrl Pts',(-45.0471384631867,0.00180683428705364,
-46.273725100927));
#34472=CARTESIAN_POINT('Ctrl Pts',(-45.0471425352043,0.00182392564630702,
-46.2742130349624));
#34473=CARTESIAN_POINT('Ctrl Pts',(-45.0471458420517,0.00183844866426805,
-46.2746246568583));
#34474=CARTESIAN_POINT('Ctrl Pts',(-45.0471491193093,0.00185294611161013,
-46.2750334800828));
#34475=CARTESIAN_POINT('Origin',(-48.7903679018718,4.,-44.5477272147525));
#34476=CARTESIAN_POINT('',(-44.9012806053458,4.,-48.4368145112785));
#34477=CARTESIAN_POINT('',(-43.6047077300919,4.,-49.7333873865323));
#34478=CARTESIAN_POINT('',(-44.9012806053458,4.,-48.4368145112785));
#34479=CARTESIAN_POINT('Ctrl Pts',(-45.0471491193093,0.00185294611161013,
-46.2750334800827));
#34480=CARTESIAN_POINT('Ctrl Pts',(-45.0471024685793,0.00164657951619665,
-46.2692140102843));
#34481=CARTESIAN_POINT('Ctrl Pts',(-45.0466809306791,0.000220053554162977,
-46.2265311890134));
#34482=CARTESIAN_POINT('Ctrl Pts',(-45.0461077679213,1.29647441628623E-5,
-46.1797598454878));
#34483=CARTESIAN_POINT('Ctrl Pts',(-45.0460284930352,2.98573545895863E-18,
-46.1722185099715));
#34484=CARTESIAN_POINT('Ctrl Pts',(-45.0460121855233,0.,-46.1707625875413));
#34485=CARTESIAN_POINT('Ctrl Pts',(-44.7142011829381,0.00185294611161013,
-46.2750334800827));
#34486=CARTESIAN_POINT('Ctrl Pts',(-44.7141856326948,0.00164657951619654,
-46.2692140102843));
#34487=CARTESIAN_POINT('Ctrl Pts',(-44.7140913997768,0.00022005355416289,
-46.2265311890134));
#34488=CARTESIAN_POINT('Ctrl Pts',(-44.7138405460215,1.29647441628478E-5,
-46.1797598454878));
#34489=CARTESIAN_POINT('Ctrl Pts',(-44.7138276408467,2.02507727125502E-18,
-46.1722185099715));
#34490=CARTESIAN_POINT('Ctrl Pts',(-44.7138222050094,0.,-46.1707625875413));
#34491=CARTESIAN_POINT('Ctrl Pts',(-44.3812532465669,0.00185294611161013,
-46.2750334800828));
#34492=CARTESIAN_POINT('Ctrl Pts',(-44.3812687968102,0.0016465795161965,
-46.2692140102843));
#34493=CARTESIAN_POINT('Ctrl Pts',(-44.3814880693913,-2.42006109825039E-5,
-46.2264061493503));
#34494=CARTESIAN_POINT('Ctrl Pts',(-44.3816312506108,0.00016460402120339,
-46.1797424783604));
#34495=CARTESIAN_POINT('Ctrl Pts',(-44.3816267886582,1.05075738695553E-18,
-46.1722185099715));
#34496=CARTESIAN_POINT('Ctrl Pts',(-44.3816322244956,0.,-46.1707625875413));
#34497=CARTESIAN_POINT('Ctrl Pts',(-44.0483053101957,0.00185294611161013,
-46.2750334800828));
#34498=CARTESIAN_POINT('Ctrl Pts',(-44.0483519609257,0.00164657951619639,
-46.2692140102843));
#34499=CARTESIAN_POINT('Ctrl Pts',(-44.0487734988259,0.000220053554162283,
-46.2265311890134));
#34500=CARTESIAN_POINT('Ctrl Pts',(-44.0493466615837,1.29647441628678E-5,
-46.1797598454878));
#34501=CARTESIAN_POINT('Ctrl Pts',(-44.0494259364698,9.6314047063189E-20,
-46.1722185099715));
#34502=CARTESIAN_POINT('Ctrl Pts',(-44.0494422439817,0.,-46.1707625875413));
#34503=CARTESIAN_POINT('',(-44.0483053101957,0.00185294611161013,-46.2750334800828));
#34504=CARTESIAN_POINT('Ctrl Pts',(-44.0483053101957,0.00185294611161013,
-46.2750334800828));
#34505=CARTESIAN_POINT('Ctrl Pts',(-44.3812532465669,0.00185294611161013,
-46.2750334800828));
#34506=CARTESIAN_POINT('Ctrl Pts',(-44.7142011829381,0.00185294611161013,
-46.2750334800827));
#34507=CARTESIAN_POINT('Ctrl Pts',(-45.0471491193093,0.00185294611161013,
-46.2750334800827));
#34508=CARTESIAN_POINT('Ctrl Pts',(-44.0483053101957,0.00185294611161058,
-46.2750334800828));
#34509=CARTESIAN_POINT('Ctrl Pts',(-44.0483090226666,0.00183652343213972,
-46.2745703659484));
#34510=CARTESIAN_POINT('Ctrl Pts',(-44.0483127824262,0.0018200291355136,
-46.2741026813164));
#34511=CARTESIAN_POINT('Ctrl Pts',(-44.0483176290461,0.0017998906188208,
-46.2735266846993));
#34512=CARTESIAN_POINT('Ctrl Pts',(-44.0483227156797,0.00177875480534672,
-46.272922163659));
#34513=CARTESIAN_POINT('Ctrl Pts',(-44.0483289966859,0.00175361200744154,
-46.2721986280875));
#34514=CARTESIAN_POINT('Ctrl Pts',(-44.0483371217799,0.00172265954511208,
-46.2712941819278));
#34515=CARTESIAN_POINT('Ctrl Pts',(-44.048345778298,0.00168968262836068,
-46.2703305802151));
#34516=CARTESIAN_POINT('Ctrl Pts',(-44.0483565245126,0.00165012867729383,
-46.2691620271535));
#34517=CARTESIAN_POINT('Ctrl Pts',(-44.0483695825273,0.00160423233980977,
-46.2677727834886));
#34518=CARTESIAN_POINT('Ctrl Pts',(-44.0483839978134,0.00155356546215882,
-46.2662391395715));
#34519=CARTESIAN_POINT('Ctrl Pts',(-44.0484012262045,0.0014952170185302,
-46.2644371217823));
#34520=CARTESIAN_POINT('Ctrl Pts',(-44.0484209571946,0.0014318755782825,
-46.2624081930856));
#34521=CARTESIAN_POINT('Ctrl Pts',(-44.0484457147017,0.00135239775434602,
-46.2598623899414));
#34522=CARTESIAN_POINT('Ctrl Pts',(-44.0484744050917,0.00126521876821268,
-46.2569605947755));
#34523=CARTESIAN_POINT('Ctrl Pts',(-44.0485055507637,0.00117763891592593,
-46.2538679066073));
#34524=CARTESIAN_POINT('Ctrl Pts',(-44.0485385798074,0.00108476312989682,
-46.2505882042891));
#34525=CARTESIAN_POINT('Ctrl Pts',(-44.0485743057099,0.000991719524367669,
-46.2471005941736));
#34526=CARTESIAN_POINT('Ctrl Pts',(-44.0486107060283,0.000905201076378148,
-46.2436166498114));
#34527=CARTESIAN_POINT('Ctrl Pts',(-44.0486382890167,0.000839640184351458,
-46.2409766290359));
#34528=CARTESIAN_POINT('Ctrl Pts',(-44.0486662443592,0.000777766532126836,
-46.2383398635846));
#34529=CARTESIAN_POINT('Ctrl Pts',(-44.0486939845841,0.000720694561437307,
-46.2357648305549));
#34530=CARTESIAN_POINT('Ctrl Pts',(-44.0487190167163,0.000669194145876824,
-46.233441180793));
#34531=CARTESIAN_POINT('Ctrl Pts',(-44.0487438668228,0.000621574660648363,
-46.2311683745643));
#34532=CARTESIAN_POINT('Ctrl Pts',(-44.0487685011858,0.00057751260431993,
-46.2289480715863));
#34533=CARTESIAN_POINT('Ctrl Pts',(-44.0487928101048,0.000534032650715443,
-46.2267571009754));
#34534=CARTESIAN_POINT('Ctrl Pts',(-44.0488168988526,0.00049399644542456,
-46.2246181983231));
#34535=CARTESIAN_POINT('Ctrl Pts',(-44.0488412714441,0.00045625393764781,
-46.2224789858338));
#34536=CARTESIAN_POINT('Ctrl Pts',(-44.0488650339742,0.000419456148745576,
-46.220393319188));
#34537=CARTESIAN_POINT('Ctrl Pts',(-44.0488891637718,0.00038468030380222,
-46.218298006353));
#34538=CARTESIAN_POINT('Ctrl Pts',(-44.0489140343552,0.000351435419317037,
-46.2161513192567));
#34539=CARTESIAN_POINT('Ctrl Pts',(-44.0489407657167,0.00031570320462769,
-46.2138440203931));
#34540=CARTESIAN_POINT('Ctrl Pts',(-44.0489683477029,0.000281787957698108,
-46.2114778723627));
#34541=CARTESIAN_POINT('Ctrl Pts',(-44.0489965895955,0.000250206967374655,
-46.2090611791433));
#34542=CARTESIAN_POINT('Ctrl Pts',(-44.0490288558276,0.000214125831553833,
-46.2063001182839));
#34543=CARTESIAN_POINT('Ctrl Pts',(-44.049061975008,0.000181169469757948,
-46.2034738288056));
#34544=CARTESIAN_POINT('Ctrl Pts',(-44.0490949331765,0.000152480845402536,
-46.2006615752138));
#34545=CARTESIAN_POINT('Ctrl Pts',(-44.049140586541,0.000112741615843626,
-46.1967660663292));
#34546=CARTESIAN_POINT('Ctrl Pts',(-44.0491858793417,8.14691463146172E-5,
-46.1929016183743));
#34547=CARTESIAN_POINT('Ctrl Pts',(-44.0492271469902,5.90616066535876E-5,
-46.1893720134754));
#34548=CARTESIAN_POINT('Ctrl Pts',(-44.0492580977266,4.22559519078155E-5,
-46.1867248098013));
#34549=CARTESIAN_POINT('Ctrl Pts',(-44.0492867430027,3.03183594507372E-5,
-46.1842697342869));
#34550=CARTESIAN_POINT('Ctrl Pts',(-44.0493118318649,2.19691435519032E-5,
-46.182113198725));
#34551=CARTESIAN_POINT('Ctrl Pts',(-44.0493328522976,1.49738430459103E-5,
-46.1803063686597));
#34552=CARTESIAN_POINT('Ctrl Pts',(-44.0493513710208,1.04521897685428E-5,
-46.1787096280762));
#34553=CARTESIAN_POINT('Ctrl Pts',(-44.0493670971357,7.39546431227645E-6,
-46.1773487225907));
#34554=CARTESIAN_POINT('Ctrl Pts',(-44.0493818826966,4.52155678414927E-6,
-46.1760692107156));
#34555=CARTESIAN_POINT('Ctrl Pts',(-44.0493941933127,2.92603171325643E-6,
-46.174998753767));
#34556=CARTESIAN_POINT('Ctrl Pts',(-44.0494042994618,1.91616332667621E-6,
-46.1741153616203));
#34557=CARTESIAN_POINT('Ctrl Pts',(-44.0494137189287,9.74912422044362E-7,
-46.17329199328));
#34558=CARTESIAN_POINT('Ctrl Pts',(-44.0494212211579,5.41797940269787E-7,
-46.1726313429966));
#34559=CARTESIAN_POINT('Ctrl Pts',(-44.0494275394041,2.92018561776075E-7,
-46.1720715563379));
#34560=CARTESIAN_POINT('Ctrl Pts',(-44.0494330489028,7.4211420916902E-8,
-46.171583423441));
#34561=CARTESIAN_POINT('Ctrl Pts',(-44.0494376626249,-2.22022958507713E-16,
-46.1711716076359));
#34562=CARTESIAN_POINT('Ctrl Pts',(-44.0494422439817,-2.22044604925031E-16,
-46.1707625875413));
#34563=CARTESIAN_POINT('Ctrl Pts',(-44.0483053101957,0.00185294611161013,
-46.2750334800828));
#34564=CARTESIAN_POINT('Ctrl Pts',(-44.0439831526635,0.020972666947357,
-46.814203289689));
#34565=CARTESIAN_POINT('Ctrl Pts',(-44.0825226081571,0.308848973617166,
-47.6898108873462));
#34566=CARTESIAN_POINT('Ctrl Pts',(-44.1731944556687,0.985587673094177,
-48.3464461826959));
#34567=CARTESIAN_POINT('Ctrl Pts',(-44.1941738241592,1.33275179473161,-48.4368145112785));
#34568=CARTESIAN_POINT('Ctrl Pts',(-44.1941738241592,1.5,-48.4368145112785));
#34569=CARTESIAN_POINT('Ctrl Pts',(-44.3812532465669,0.00185294611161013,
-46.2750334800828));
#34570=CARTESIAN_POINT('Ctrl Pts',(-44.3798125273895,0.0209726669473568,
-46.814203289689));
#34571=CARTESIAN_POINT('Ctrl Pts',(-44.392659012554,0.308848973617166,-47.6898108873462));
#34572=CARTESIAN_POINT('Ctrl Pts',(-44.4228829617246,0.985587673094178,
-48.3464461826959));
#34573=CARTESIAN_POINT('Ctrl Pts',(-44.4298760845547,1.33275179473162,-48.4368145112785));
#34574=CARTESIAN_POINT('Ctrl Pts',(-44.4298760845547,1.5,-48.4368145112785));
#34575=CARTESIAN_POINT('Ctrl Pts',(-44.7142011829381,0.00185294611161013,
-46.2750334800827));
#34576=CARTESIAN_POINT('Ctrl Pts',(-44.7156419021155,0.0209726669473567,
-46.8142032896889));
#34577=CARTESIAN_POINT('Ctrl Pts',(-44.7027954169509,0.308848973617164,
-47.6898108873462));
#34578=CARTESIAN_POINT('Ctrl Pts',(-44.6725714677804,0.985587673094178,
-48.3464461826959));
#34579=CARTESIAN_POINT('Ctrl Pts',(-44.6655783449502,1.33275179473162,-48.4368145112785));
#34580=CARTESIAN_POINT('Ctrl Pts',(-44.6655783449502,1.5,-48.4368145112785));
#34581=CARTESIAN_POINT('Ctrl Pts',(-45.0471491193093,0.00185294611161013,
-46.2750334800827));
#34582=CARTESIAN_POINT('Ctrl Pts',(-45.0514712768415,0.0209726669473565,
-46.8142032896889));
#34583=CARTESIAN_POINT('Ctrl Pts',(-45.0129318213479,0.308848973617163,
-47.6898108873462));
#34584=CARTESIAN_POINT('Ctrl Pts',(-44.9222599738363,0.985587673094179,
-48.3464461826959));
#34585=CARTESIAN_POINT('Ctrl Pts',(-44.9012806053458,1.33275179473162,-48.4368145112785));
#34586=CARTESIAN_POINT('Ctrl Pts',(-44.9012806053458,1.5,-48.4368145112785));
#34587=CARTESIAN_POINT('',(-44.1941738241592,1.5,-48.4368145112785));
#34588=CARTESIAN_POINT('',(-44.9012806053458,1.5,-48.4368145112785));
#34589=CARTESIAN_POINT('Ctrl Pts',(-44.1941738241592,1.5,-48.4368145112785));
#34590=CARTESIAN_POINT('Ctrl Pts',(-44.1941738241592,1.33275179473161,-48.4368145112785));
#34591=CARTESIAN_POINT('Ctrl Pts',(-44.1731944556687,0.985587673094177,
-48.3464461826959));
#34592=CARTESIAN_POINT('Ctrl Pts',(-44.0825226081571,0.308848973617166,
-47.6898108873462));
#34593=CARTESIAN_POINT('Ctrl Pts',(-44.0439831526635,0.020972666947357,
-46.814203289689));
#34594=CARTESIAN_POINT('Ctrl Pts',(-44.0483053101957,0.00185294611161013,
-46.2750334800828));
#34595=CARTESIAN_POINT('Origin',(-44.5477272147525,4.,-48.4368145112785));
#34596=CARTESIAN_POINT('',(-44.1941738241592,4.,-48.4368145112785));
#34597=CARTESIAN_POINT('',(-22.2738636073762,4.,-48.4368145112785));
#34598=CARTESIAN_POINT('',(-44.1941738241592,4.,-48.4368145112785));
#34599=CARTESIAN_POINT('Origin',(-26.3988636073762,1.5,-28.5201839509359));
#34600=CARTESIAN_POINT('',(-31.0449275599944,1.5,-35.2875682471136));
#34601=CARTESIAN_POINT('',(-25.3382034355964,1.5,-29.5808441227157));
#34602=CARTESIAN_POINT('Ctrl Pts',(-31.0952102098472,0.,-33.2165305534069));
#34603=CARTESIAN_POINT('Ctrl Pts',(-31.0951683510534,1.11734401589392E-19,
-33.2190692967299));
#34604=CARTESIAN_POINT('Ctrl Pts',(-31.0951264183426,3.32975363939714E-6,
-33.2216080407998));
#34605=CARTESIAN_POINT('Ctrl Pts',(-31.0915543966548,0.000569671234466166,
-33.4374895579288));
#34606=CARTESIAN_POINT('Ctrl Pts',(-31.0874717825085,0.024650660129702,
-33.6519250591448));
#34607=CARTESIAN_POINT('Ctrl Pts',(-31.0788092838543,0.119724494999934,
-34.0573511387189));
#34608=CARTESIAN_POINT('Ctrl Pts',(-31.0742145020816,0.188992076600158,
-34.2510845845319));
#34609=CARTESIAN_POINT('Ctrl Pts',(-31.0647171688648,0.382511576258832,
-34.6214706148708));
#34610=CARTESIAN_POINT('Ctrl Pts',(-31.0597601262273,0.510857073213101,
-34.7982799030232));
#34611=CARTESIAN_POINT('Ctrl Pts',(-31.0522501584557,0.790024881159197,
-35.0535067624131));
#34612=CARTESIAN_POINT('Ctrl Pts',(-31.0494412598632,0.927714535375556,
-35.1443641805612));
#34613=CARTESIAN_POINT('Ctrl Pts',(-31.0458492854634,1.2139998648115,-35.2589537310755));
#34614=CARTESIAN_POINT('Ctrl Pts',(-31.0449275599944,1.35542940125327,-35.2875682471136));
#34615=CARTESIAN_POINT('Ctrl Pts',(-31.0449275599944,1.5,-35.2875682471136));
#34616=CARTESIAN_POINT('Origin',(-44.5477272147525,4.,-48.7903679018718));
#34617=CARTESIAN_POINT('',(-31.0449275599944,4.,-35.2875682471136));
#34618=CARTESIAN_POINT('',(-25.3382034355964,4.,-29.5808441227157));
#34619=CARTESIAN_POINT('',(-31.0449275599944,4.,-35.2875682471136));
#34620=CARTESIAN_POINT('Origin',(-53.2,0.25,0.));
#34621=CARTESIAN_POINT('',(-58.95,0.25,-7.04171909509728E-16));
#34622=CARTESIAN_POINT('Origin',(53.2,0.25,0.));
#34623=CARTESIAN_POINT('',(47.45,0.25,-7.04171909509728E-16));
#34624=CARTESIAN_POINT('Origin',(44.5477272147525,4.,-48.4368145112785));
#34625=CARTESIAN_POINT('',(44.1941738241592,4.,-48.4368145112785));
#34626=CARTESIAN_POINT('',(44.9012806053458,4.,-48.4368145112785));
#34627=CARTESIAN_POINT('',(22.2738636073762,4.,-48.4368145112785));
#34628=CARTESIAN_POINT('',(44.9012806053458,1.5,-48.4368145112785));
#34629=CARTESIAN_POINT('',(44.9012806053458,4.,-48.4368145112785));
#34630=CARTESIAN_POINT('',(44.1941738241592,1.5,-48.4368145112785));
#34631=CARTESIAN_POINT('',(44.9012806053458,1.5,-48.4368145112785));
#34632=CARTESIAN_POINT('',(44.1941738241592,4.,-48.4368145112785));
#34633=CARTESIAN_POINT('Origin',(45.4316106912357,1.5,-47.5529310347953));
#34634=CARTESIAN_POINT('',(45.6083873865323,0.500000000000005,-47.729707730092));
#34635=CARTESIAN_POINT('',(45.6083873865323,0.500000000000005,-47.729707730092));
#34636=CARTESIAN_POINT('Origin',(45.2548339959391,1.5,-47.3761543394987));
#34637=CARTESIAN_POINT('Origin',(45.6083873865323,1.5,-47.729707730092));
#34638=CARTESIAN_POINT('Origin',(41.3066106912357,0.25,-51.6779310347953));
#34639=CARTESIAN_POINT('',(47.729707730092,0.5,-45.6083873865323));
#34640=CARTESIAN_POINT('',(47.729707730092,0.5,-45.6083873865323));
#34641=CARTESIAN_POINT('',(41.4833873865323,0.5,-51.854707730092));
#34642=CARTESIAN_POINT('Origin',(47.5529310347953,1.5,-45.4316106912357));
#34643=CARTESIAN_POINT('',(48.4368145112785,1.5,-44.9012806053458));
#34644=CARTESIAN_POINT('',(48.4368145112785,1.5,-44.1941738241592));
#34645=CARTESIAN_POINT('',(48.4368145112785,1.5,-44.9012806053458));
#34646=CARTESIAN_POINT('Origin',(47.3761543394987,1.5,-45.254833995939));
#34647=CARTESIAN_POINT('Origin',(47.729707730092,1.5,-45.6083873865323));
#34648=CARTESIAN_POINT('Origin',(48.4368145112785,4.,-44.5477272147525));
#34649=CARTESIAN_POINT('',(48.4368145112785,4.,-44.9012806053458));
#34650=CARTESIAN_POINT('',(48.4368145112785,4.,-44.1941738241592));
#34651=CARTESIAN_POINT('',(48.4368145112785,4.,-30.5238636073763));
#34652=CARTESIAN_POINT('',(48.4368145112785,4.,-44.1941738241592));
#34653=CARTESIAN_POINT('',(48.4368145112785,4.,-44.9012806053458));
#34654=CARTESIAN_POINT('Origin',(44.5477272147525,4.,-48.7903679018718));
#34655=CARTESIAN_POINT('',(41.4833873865323,4.,-51.854707730092));
#34656=CARTESIAN_POINT('Origin',(0.,2.5,0.));
#34657=CARTESIAN_POINT('',(-13.3416640641263,4.,43.5));
#34658=CARTESIAN_POINT('',(-17.7974717305577,2.5,43.5));
#34659=CARTESIAN_POINT('Ctrl Pts',(-17.7974717305577,2.5,43.5));
#34660=CARTESIAN_POINT('Ctrl Pts',(-17.7974717305577,2.55909958962217,43.5));
#34661=CARTESIAN_POINT('Ctrl Pts',(-17.7856223944691,2.62902218815019,43.5));
#34662=CARTESIAN_POINT('Ctrl Pts',(-17.7453636557976,2.75139686483799,43.5));
#34663=CARTESIAN_POINT('Ctrl Pts',(-17.706168118457,2.82532121452828,43.5));
#34664=CARTESIAN_POINT('Ctrl Pts',(-17.5359812657224,3.06819459814041,43.5));
#34665=CARTESIAN_POINT('Ctrl Pts',(-17.3144913010137,3.22642942545082,43.5));
#34666=CARTESIAN_POINT('Ctrl Pts',(-16.5770721718092,3.62923551489079,43.5));
#34667=CARTESIAN_POINT('Ctrl Pts',(-15.9375248631358,3.77596647975076,43.5));
#34668=CARTESIAN_POINT('Ctrl Pts',(-14.6274773462457,3.96791177668935,43.5));
#34669=CARTESIAN_POINT('Ctrl Pts',(-13.9550874901819,4.,43.5));
#34670=CARTESIAN_POINT('Ctrl Pts',(-13.3416640641263,4.,43.5));
#34671=CARTESIAN_POINT('',(17.7974717305577,2.5,43.5));
#34672=CARTESIAN_POINT('Origin',(0.,2.5,0.));
#34673=CARTESIAN_POINT('',(13.3416640641263,4.,43.5));
#34674=CARTESIAN_POINT('Ctrl Pts',(13.3416640641263,4.,43.5));
#34675=CARTESIAN_POINT('Ctrl Pts',(13.9550874901819,4.,43.5));
#34676=CARTESIAN_POINT('Ctrl Pts',(14.6274773462457,3.96791177668935,43.5));
#34677=CARTESIAN_POINT('Ctrl Pts',(15.9375248631358,3.77596647975076,43.5));
#34678=CARTESIAN_POINT('Ctrl Pts',(16.5770721718093,3.62923551489079,43.5));
#34679=CARTESIAN_POINT('Ctrl Pts',(17.3144913010137,3.22642942545082,43.5));
#34680=CARTESIAN_POINT('Ctrl Pts',(17.5359812657224,3.06819459814041,43.5));
#34681=CARTESIAN_POINT('Ctrl Pts',(17.706168118457,2.82532121452828,43.5));
#34682=CARTESIAN_POINT('Ctrl Pts',(17.7453636557976,2.75139686483799,43.5));
#34683=CARTESIAN_POINT('Ctrl Pts',(17.7856223944691,2.62902218815019,43.5));
#34684=CARTESIAN_POINT('Ctrl Pts',(17.7974717305577,2.55909958962217,43.5));
#34685=CARTESIAN_POINT('Ctrl Pts',(17.7974717305577,2.5,43.5));
#34686=CARTESIAN_POINT('Origin',(0.,4.,0.));
#34687=CARTESIAN_POINT('Origin',(0.,4.,0.));
#34688=CARTESIAN_POINT('',(-17.7974717305577,1.5,43.5));
#34689=CARTESIAN_POINT('',(-17.7974717305577,4.,43.5));
#34690=CARTESIAN_POINT('',(17.7974717305577,1.5,43.5));
#34691=CARTESIAN_POINT('Origin',(0.,1.5,0.));
#34692=CARTESIAN_POINT('',(17.7974717305577,4.,43.5));
#34693=CARTESIAN_POINT('Origin',(-53.2,1.5,0.));
#34694=CARTESIAN_POINT('',(-46.2240601503759,1.5,8.50507279301165));
#34695=CARTESIAN_POINT('Ctrl Pts',(-45.209022556391,0.,5.13753632549025));
#34696=CARTESIAN_POINT('Ctrl Pts',(-45.2101706901705,-1.40306832022943E-18,
5.14245954784658));
#34697=CARTESIAN_POINT('Ctrl Pts',(-45.2113202904355,2.87874308356214E-6,
5.1473824373595));
#34698=CARTESIAN_POINT('Ctrl Pts',(-45.3805806089602,0.000852747696532382,
5.87122802959633));
#34699=CARTESIAN_POINT('Ctrl Pts',(-45.5407068125259,0.0644575560773281,
6.42770684158595));
#34700=CARTESIAN_POINT('Ctrl Pts',(-45.7992896021911,0.262676028338797,
7.27728490933266));
#34701=CARTESIAN_POINT('Ctrl Pts',(-45.9058399421765,0.391768785578365,
7.59761029794946));
#34702=CARTESIAN_POINT('Ctrl Pts',(-46.0437392091658,0.637700968927193,
8.00108322240395));
#34703=CARTESIAN_POINT('Ctrl Pts',(-46.095986299131,0.7544352578638,8.14964878644437));
#34704=CARTESIAN_POINT('Ctrl Pts',(-46.165500553065,0.987918955923497,8.34412682404574));
#34705=CARTESIAN_POINT('Ctrl Pts',(-46.1888166753861,1.09129381988889,8.40843236441884));
#34706=CARTESIAN_POINT('Ctrl Pts',(-46.2170785613611,1.29969233992949,8.48604609926929));
#34707=CARTESIAN_POINT('Ctrl Pts',(-46.2240601503759,1.39848091468836,8.50507279301165));
#34708=CARTESIAN_POINT('Ctrl Pts',(-46.2240601503759,1.5,8.50507279301165));
#34709=CARTESIAN_POINT('',(-58.,1.5,9.8974744253269));
#34710=CARTESIAN_POINT('Origin',(-53.2,1.5,0.));
#34711=CARTESIAN_POINT('Ctrl Pts',(-59.5,0.,7.11055553385247));
#34712=CARTESIAN_POINT('Ctrl Pts',(-59.4982621111229,-1.43714039392157E-18,
7.11441720740624));
#34713=CARTESIAN_POINT('Ctrl Pts',(-59.4965230425191,3.02025636744488E-6,
7.11827835650607));
#34714=CARTESIAN_POINT('Ctrl Pts',(-59.2998658347014,0.000687024107797437,
7.5545495242394));
#34715=CARTESIAN_POINT('Ctrl Pts',(-59.0848279111169,0.0390861404131355,
7.99027457435746));
#34716=CARTESIAN_POINT('Ctrl Pts',(-58.6790205873,0.227280698650663,8.75389357006342));
#34717=CARTESIAN_POINT('Ctrl Pts',(-58.5106474320197,0.353869330585226,
9.04860693524616));
#34718=CARTESIAN_POINT('Ctrl Pts',(-58.2889293801926,0.605541836240553,
9.4260831564163));
#34719=CARTESIAN_POINT('Ctrl Pts',(-58.2055841166437,0.725339698576898,
9.56428617469307));
#34720=CARTESIAN_POINT('Ctrl Pts',(-58.0942335303233,0.966223567273987,
9.74614959515893));
#34721=CARTESIAN_POINT('Ctrl Pts',(-58.0567637695508,1.07370986494963,9.80652098494185));
#34722=CARTESIAN_POINT('Ctrl Pts',(-58.01124521301,1.29080573116058,9.87956234691206));
#34723=CARTESIAN_POINT('Ctrl Pts',(-58.,1.3939909411326,9.89747442532689));
#34724=CARTESIAN_POINT('Ctrl Pts',(-58.,1.5,9.89747442532689));
#34725=CARTESIAN_POINT('Origin',(0.,1.5,0.));
#34726=CARTESIAN_POINT('',(-30.8017856625229,1.5,35.5));
#34727=CARTESIAN_POINT('Ctrl Pts',(-26.4811253537307,0.,37.));
#34728=CARTESIAN_POINT('Ctrl Pts',(-26.4867878946248,1.06044817773062E-17,
36.9981824187244));
#34729=CARTESIAN_POINT('Ctrl Pts',(-26.4924502779527,3.30360139702406E-6,
36.9963643050345));
#34730=CARTESIAN_POINT('Ctrl Pts',(-27.6012019204162,0.00129824004375969,
36.6402452052783));
#34731=CARTESIAN_POINT('Ctrl Pts',(-28.6022785210026,0.127864463880204,
36.2954324644459));
#34732=CARTESIAN_POINT('Ctrl Pts',(-29.7527298503777,0.479548357456909,
35.8858963683834));
#34733=CARTESIAN_POINT('Ctrl Pts',(-30.0640351469117,0.619696008492602,
35.7724767899835));
#34734=CARTESIAN_POINT('Ctrl Pts',(-30.4199450706296,0.856752956966091,
35.6417681188669));
#34735=CARTESIAN_POINT('Ctrl Pts',(-30.5405284008673,0.955292659882126,
35.5971805278559));
#34736=CARTESIAN_POINT('Ctrl Pts',(-30.6877287941394,1.1384738095481,35.5425226152298));
#34737=CARTESIAN_POINT('Ctrl Pts',(-30.7342206529605,1.21379195435448,35.525203642034));
#34738=CARTESIAN_POINT('Ctrl Pts',(-30.7885863901991,1.36171319479544,35.5049304586301));
#34739=CARTESIAN_POINT('Ctrl Pts',(-30.8017856625229,1.42978275763033,35.5));
#34740=CARTESIAN_POINT('Ctrl Pts',(-30.8017856625229,1.5,35.5));
#34741=CARTESIAN_POINT('Origin',(0.,1.5,0.));
#34742=CARTESIAN_POINT('Origin',(-36.,1.5,13.5));
#34743=CARTESIAN_POINT('',(-58.,1.5,13.5));
#34744=CARTESIAN_POINT('Origin',(-59.5,1.5,13.5));
#34745=CARTESIAN_POINT('',(-36.,1.5,35.5));
#34746=CARTESIAN_POINT('Origin',(-36.,1.5,13.5));
#34747=CARTESIAN_POINT('Origin',(-36.,1.5,37.));
#34748=CARTESIAN_POINT('Origin',(-18.,1.5,37.));
#34749=CARTESIAN_POINT('',(-18.,1.5,35.5));
#34750=CARTESIAN_POINT('Origin',(-59.5,1.5,-31.5));
#34751=CARTESIAN_POINT('',(-58.,1.5,-31.5));
#34752=CARTESIAN_POINT('Origin',(0.,4.,0.));
#34753=CARTESIAN_POINT('',(-30.8017856625229,4.,35.5));
#34754=CARTESIAN_POINT('',(-30.8017856625229,4.,35.5));
#34755=CARTESIAN_POINT('',(-46.2240601503759,4.,8.50507279301165));
#34756=CARTESIAN_POINT('Origin',(0.,4.,0.));
#34757=CARTESIAN_POINT('',(-46.2240601503759,4.,8.50507279301165));
#34758=CARTESIAN_POINT('Origin',(-36.,0.,35.5));
#34759=CARTESIAN_POINT('',(-36.,4.,35.5));
#34760=CARTESIAN_POINT('',(-36.,0.,35.5));
#34761=CARTESIAN_POINT('',(36.,4.,35.5));
#34762=CARTESIAN_POINT('Origin',(-36.,0.,13.5));
#34763=CARTESIAN_POINT('',(-58.,4.,13.5));
#34764=CARTESIAN_POINT('',(-58.,0.,13.5));
#34765=CARTESIAN_POINT('Origin',(-36.,4.,13.5));
#34766=CARTESIAN_POINT('Origin',(0.,1.5,0.));
#34767=CARTESIAN_POINT('',(46.2240601503759,1.5,8.50507279301165));
#34768=CARTESIAN_POINT('Ctrl Pts',(45.209022556391,0.,5.1375363254903));
#34769=CARTESIAN_POINT('Ctrl Pts',(45.2102521007232,1.11258750894249E-19,
5.14280863804894));
#34770=CARTESIAN_POINT('Ctrl Pts',(45.2114833270665,3.30146167889055E-6,
5.14808056967696));
#34771=CARTESIAN_POINT('Ctrl Pts',(45.3784738591765,0.000901308928852578,
5.86208365506188));
#34772=CARTESIAN_POINT('Ctrl Pts',(45.5364437851314,0.0627444670134214,
6.4126471717855));
#34773=CARTESIAN_POINT('Ctrl Pts',(45.7956313154401,0.258490073791997,7.2662018107722));
#34774=CARTESIAN_POINT('Ctrl Pts',(45.9037816258573,0.388566620441501,7.59150909299489));
#34775=CARTESIAN_POINT('Ctrl Pts',(46.043055046971,0.636193465569317,7.99912982559317));
#34776=CARTESIAN_POINT('Ctrl Pts',(46.0956128185241,0.753321114945002,8.14859884634578));
#34777=CARTESIAN_POINT('Ctrl Pts',(46.1654106238969,0.987526374219774,8.34387849941688));
#34778=CARTESIAN_POINT('Ctrl Pts',(46.1887788399396,1.09104391483163,8.40832834536188));
#34779=CARTESIAN_POINT('Ctrl Pts',(46.2170749275856,1.29964148682512,8.48603621443855));
#34780=CARTESIAN_POINT('Ctrl Pts',(46.2240601503759,1.39845449738161,8.50507279301165));
#34781=CARTESIAN_POINT('Ctrl Pts',(46.2240601503759,1.5,8.50507279301165));
#34782=CARTESIAN_POINT('',(30.8017856625229,1.5,35.5));
#34783=CARTESIAN_POINT('Origin',(0.,1.5,0.));
#34784=CARTESIAN_POINT('Ctrl Pts',(26.4811253537307,0.,37.));
#34785=CARTESIAN_POINT('Ctrl Pts',(26.4867878946292,1.11294754654022E-19,
36.998182418723));
#34786=CARTESIAN_POINT('Ctrl Pts',(26.4924502779482,3.30360139191886E-6,
36.996364305036));
#34787=CARTESIAN_POINT('Ctrl Pts',(27.6012019219699,0.00129824004556856,
36.6402452047772));
#34788=CARTESIAN_POINT('Ctrl Pts',(28.6022785220106,0.127864464188313,36.2954324640871));
#34789=CARTESIAN_POINT('Ctrl Pts',(29.7527298503796,0.479548357457492,35.8858963683827));
#34790=CARTESIAN_POINT('Ctrl Pts',(30.0640351469129,0.619696008493419,35.7724767899831));
#34791=CARTESIAN_POINT('Ctrl Pts',(30.4199450706296,0.856752956966088,35.6417681188669));
#34792=CARTESIAN_POINT('Ctrl Pts',(30.5405284008673,0.955292659882133,35.5971805278559));
#34793=CARTESIAN_POINT('Ctrl Pts',(30.6877287941394,1.13847380954807,35.5425226152298));
#34794=CARTESIAN_POINT('Ctrl Pts',(30.7342206529605,1.21379195435447,35.525203642034));
#34795=CARTESIAN_POINT('Ctrl Pts',(30.7885863901995,1.3617131947964,35.5049304586299));
#34796=CARTESIAN_POINT('Ctrl Pts',(30.8017856625229,1.42978275763078,35.5));
#34797=CARTESIAN_POINT('Ctrl Pts',(30.8017856625229,1.5,35.5));
#34798=CARTESIAN_POINT('Origin',(53.2,1.5,0.));
#34799=CARTESIAN_POINT('',(58.,1.5,9.8974744253269));
#34800=CARTESIAN_POINT('Ctrl Pts',(59.5,0.,7.11055553385247));
#34801=CARTESIAN_POINT('Ctrl Pts',(59.4982621111229,-1.43714039392157E-18,
7.11441720740624));
#34802=CARTESIAN_POINT('Ctrl Pts',(59.4965230425191,3.02025636744488E-6,
7.11827835650607));
#34803=CARTESIAN_POINT('Ctrl Pts',(59.2998658347014,0.000687024107797401,
7.55454952423938));
#34804=CARTESIAN_POINT('Ctrl Pts',(59.0848279111169,0.0390861404131368,
7.99027457435745));
#34805=CARTESIAN_POINT('Ctrl Pts',(58.6790205873002,0.227280698650583,8.75389357006309));
#34806=CARTESIAN_POINT('Ctrl Pts',(58.5106474320198,0.353869330585071,9.04860693524593));
#34807=CARTESIAN_POINT('Ctrl Pts',(58.2889293801926,0.605541836240555,9.42608315641631));
#34808=CARTESIAN_POINT('Ctrl Pts',(58.2055841166437,0.725339698576898,9.56428617469307));
#34809=CARTESIAN_POINT('Ctrl Pts',(58.0942335303233,0.966223567273987,9.74614959515893));
#34810=CARTESIAN_POINT('Ctrl Pts',(58.0567637695508,1.07370986494963,9.80652098494185));
#34811=CARTESIAN_POINT('Ctrl Pts',(58.01124521301,1.29080573116058,9.87956234691206));
#34812=CARTESIAN_POINT('Ctrl Pts',(58.,1.3939909411326,9.89747442532689));
#34813=CARTESIAN_POINT('Ctrl Pts',(58.,1.5,9.89747442532689));
#34814=CARTESIAN_POINT('Origin',(53.2,1.5,0.));
#34815=CARTESIAN_POINT('Origin',(36.,1.5,13.5));
#34816=CARTESIAN_POINT('',(36.,1.5,35.5));
#34817=CARTESIAN_POINT('Origin',(36.,1.5,37.));
#34818=CARTESIAN_POINT('',(58.,1.5,13.5));
#34819=CARTESIAN_POINT('Origin',(36.,1.5,13.5));
#34820=CARTESIAN_POINT('Origin',(59.5,1.5,13.5));
#34821=CARTESIAN_POINT('Origin',(59.5,1.5,-1.5));
#34822=CARTESIAN_POINT('',(58.,1.5,-1.5));
#34823=CARTESIAN_POINT('Origin',(-18.,1.5,37.));
#34824=CARTESIAN_POINT('',(-18.,1.5,35.5));
#34825=CARTESIAN_POINT('Origin',(53.2,4.,0.));
#34826=CARTESIAN_POINT('',(58.,4.,9.8974744253269));
#34827=CARTESIAN_POINT('',(58.,4.,9.8974744253269));
#34828=CARTESIAN_POINT('',(46.2240601503759,4.,8.50507279301165));
#34829=CARTESIAN_POINT('Origin',(53.2,4.,0.));
#34830=CARTESIAN_POINT('',(46.2240601503759,4.,8.50507279301165));
#34831=CARTESIAN_POINT('Origin',(58.,0.,13.5));
#34832=CARTESIAN_POINT('',(58.,4.,13.5));
#34833=CARTESIAN_POINT('',(58.,0.,13.5));
#34834=CARTESIAN_POINT('',(58.,4.,-46.5));
#34835=CARTESIAN_POINT('Origin',(36.,0.,13.5));
#34836=CARTESIAN_POINT('',(36.,4.,35.5));
#34837=CARTESIAN_POINT('',(36.,0.,35.5));
#34838=CARTESIAN_POINT('Origin',(36.,4.,13.5));
#34839=CARTESIAN_POINT('Origin',(0.,1.5,0.));
#34840=CARTESIAN_POINT('Ctrl Pts',(17.7974717305574,1.5,43.5000000000001));
#34841=CARTESIAN_POINT('Ctrl Pts',(17.7974717305574,1.3081363470698,43.5000000000001));
#34842=CARTESIAN_POINT('Ctrl Pts',(17.7902374021495,1.11830736311257,43.4631927808952));
#34843=CARTESIAN_POINT('Ctrl Pts',(17.7620064094937,0.761470147690042,43.3198100779987));
#34844=CARTESIAN_POINT('Ctrl Pts',(17.7411731135178,0.598404516851343,43.2140759917526));
#34845=CARTESIAN_POINT('Ctrl Pts',(17.6880641128075,0.318992028184976,42.9452704489042));
#34846=CARTESIAN_POINT('Ctrl Pts',(17.6560897895307,0.206345030833379,42.7837511882912));
#34847=CARTESIAN_POINT('Ctrl Pts',(17.6020279405521,0.0861702418769968,
42.5115766866022));
#34848=CARTESIAN_POINT('Ctrl Pts',(17.5824878665501,0.0544158735673595,
42.4133539775058));
#34849=CARTESIAN_POINT('Ctrl Pts',(17.5423727024711,0.0114992072454748,
42.2120624504891));
#34850=CARTESIAN_POINT('Ctrl Pts',(17.5218884486073,0.000464895865378814,
42.1094502117176));
#34851=CARTESIAN_POINT('Ctrl Pts',(17.5008757674563,4.79373185133258E-6,
42.00437891946));
#34852=CARTESIAN_POINT('Ctrl Pts',(17.500437891852,9.05593823628022E-17,
42.0021894592601));
#34853=CARTESIAN_POINT('Ctrl Pts',(17.5,0.,42.0000000000001));
#34854=CARTESIAN_POINT('Ctrl Pts',(-17.5,0.,42.));
#34855=CARTESIAN_POINT('Ctrl Pts',(-17.500437891852,1.3406571373437E-19,
42.0021894592601));
#34856=CARTESIAN_POINT('Ctrl Pts',(-17.5008757674563,4.79373185123263E-6,
42.0043789194599));
#34857=CARTESIAN_POINT('Ctrl Pts',(-17.5218884486073,0.000464895865378844,
42.1094502117176));
#34858=CARTESIAN_POINT('Ctrl Pts',(-17.5423727024711,0.0114992072454764,
42.2120624504891));
#34859=CARTESIAN_POINT('Ctrl Pts',(-17.5824878665501,0.0544158735673544,
42.4133539775058));
#34860=CARTESIAN_POINT('Ctrl Pts',(-17.6020279405521,0.0861702418769902,
42.5115766866022));
#34861=CARTESIAN_POINT('Ctrl Pts',(-17.6560897895307,0.206345030833382,
42.7837511882912));
#34862=CARTESIAN_POINT('Ctrl Pts',(-17.6880641128075,0.31899202818498,42.9452704489042));
#34863=CARTESIAN_POINT('Ctrl Pts',(-17.7411731135178,0.598404516851343,
43.2140759917526));
#34864=CARTESIAN_POINT('Ctrl Pts',(-17.7620064094937,0.761470147690042,
43.3198100779987));
#34865=CARTESIAN_POINT('Ctrl Pts',(-17.7902374021495,1.11830736311257,43.4631927808952));
#34866=CARTESIAN_POINT('Ctrl Pts',(-17.7974717305574,1.3081363470698,43.5000000000001));
#34867=CARTESIAN_POINT('Ctrl Pts',(-17.7974717305574,1.5,43.5000000000001));
#34868=CARTESIAN_POINT('Origin',(0.,1.5,0.));
#34869=CARTESIAN_POINT('',(31.0449275599944,1.5,-35.2875682471136));
#34870=CARTESIAN_POINT('Origin',(0.,1.5,0.));
#34871=CARTESIAN_POINT('Ctrl Pts',(31.0952102098472,0.,-33.2165305534069));
#34872=CARTESIAN_POINT('Ctrl Pts',(31.0951696964714,-1.0480047872591E-17,
-33.2189876968878));
#34873=CARTESIAN_POINT('Ctrl Pts',(31.0951291138549,3.1191448844996E-6,
-33.2214448410094));
#34874=CARTESIAN_POINT('Ctrl Pts',(31.0915518419005,0.000552123420194366,
-33.4376681173871));
#34875=CARTESIAN_POINT('Ctrl Pts',(31.0874603040868,0.0247093974684173,
-33.6525355816948));
#34876=CARTESIAN_POINT('Ctrl Pts',(31.0787526147422,0.120411269801602,-34.0599327360631));
#34877=CARTESIAN_POINT('Ctrl Pts',(31.0741165440007,0.190507175290616,-34.2551775861872));
#34878=CARTESIAN_POINT('Ctrl Pts',(31.0646128476165,0.385154103985276,-34.6252458975057));
#34879=CARTESIAN_POINT('Ctrl Pts',(31.0596930143797,0.513035438790037,-34.8006041636678));
#34880=CARTESIAN_POINT('Ctrl Pts',(31.0522277771702,0.791102236957407,-35.0542336624389));
#34881=CARTESIAN_POINT('Ctrl Pts',(31.04943124825,0.9284220413215,-35.1446849201549));
#34882=CARTESIAN_POINT('Ctrl Pts',(31.0458481634946,1.21416954975876,-35.2589883222484));
#34883=CARTESIAN_POINT('Ctrl Pts',(31.0449275599943,1.35551696906064,-35.2875682471137));
#34884=CARTESIAN_POINT('Ctrl Pts',(31.0449275599943,1.5,-35.2875682471137));
#34885=CARTESIAN_POINT('Origin',(0.,4.,0.));
#34886=CARTESIAN_POINT('',(31.0449275599944,4.,-35.2875682471136));
#34887=CARTESIAN_POINT('Origin',(0.,4.,0.));
#34888=CARTESIAN_POINT('',(31.0449275599944,4.,-35.2875682471136));
#34889=CARTESIAN_POINT('Origin',(-53.2,1.5,0.));
#34890=CARTESIAN_POINT('',(-58.,1.5,-9.8974744253269));
#34891=CARTESIAN_POINT('Ctrl Pts',(-58.,1.5,-9.89747442532689));
#34892=CARTESIAN_POINT('Ctrl Pts',(-58.,1.3939909411326,-9.89747442532689));
#34893=CARTESIAN_POINT('Ctrl Pts',(-58.01124521301,1.29080573116058,-9.87956234691206));
#34894=CARTESIAN_POINT('Ctrl Pts',(-58.0567637695508,1.07370986494962,-9.80652098494185));
#34895=CARTESIAN_POINT('Ctrl Pts',(-58.0942335303233,0.966223567273955,
-9.7461495951589));
#34896=CARTESIAN_POINT('Ctrl Pts',(-58.2055841166437,0.725339698576908,
-9.56428617469307));
#34897=CARTESIAN_POINT('Ctrl Pts',(-58.2889293801925,0.605541836240571,
-9.42608315641633));
#34898=CARTESIAN_POINT('Ctrl Pts',(-58.5106474320197,0.3538693305852,-9.04860693524612));
#34899=CARTESIAN_POINT('Ctrl Pts',(-58.6790205873,0.22728069865065,-8.75389357006336));
#34900=CARTESIAN_POINT('Ctrl Pts',(-59.0848279111169,0.0390861404131358,
-7.99027457435745));
#34901=CARTESIAN_POINT('Ctrl Pts',(-59.2998658347014,0.000687024107797407,
-7.55454952423938));
#34902=CARTESIAN_POINT('Ctrl Pts',(-59.4965230425191,3.02025636744469E-6,
-7.11827835650607));
#34903=CARTESIAN_POINT('Ctrl Pts',(-59.4982621111229,-1.43714039392162E-18,
-7.11441720740624));
#34904=CARTESIAN_POINT('Ctrl Pts',(-59.5,0.,-7.11055553385247));
#34905=CARTESIAN_POINT('',(-46.2240601503759,1.5,-8.50507279301165));
#34906=CARTESIAN_POINT('Origin',(-53.2,1.5,0.));
#34907=CARTESIAN_POINT('Ctrl Pts',(-45.209022556391,0.,-5.13753632549022));
#34908=CARTESIAN_POINT('Ctrl Pts',(-45.2101706901698,-1.40306831947151E-18,
-5.1424595478439));
#34909=CARTESIAN_POINT('Ctrl Pts',(-45.2113202904361,2.87874308667369E-6,
-5.14738243736215));
#34910=CARTESIAN_POINT('Ctrl Pts',(-45.3805806080453,0.000852747691942822,
-5.87122802568613));
#34911=CARTESIAN_POINT('Ctrl Pts',(-45.5407068116734,0.0644575554238702,
-6.42770683878517));
#34912=CARTESIAN_POINT('Ctrl Pts',(-45.7992896021911,0.262676028338764,
-7.2772849093325));
#34913=CARTESIAN_POINT('Ctrl Pts',(-45.9058399421765,0.391768785578303,
-7.59761029794935));
#34914=CARTESIAN_POINT('Ctrl Pts',(-46.0437392091658,0.637700968927232,
-8.001083222404));
#34915=CARTESIAN_POINT('Ctrl Pts',(-46.095986299131,0.754435257863824,-8.14964878644436));
#34916=CARTESIAN_POINT('Ctrl Pts',(-46.165500553065,0.987918955923379,-8.34412682404563));
#34917=CARTESIAN_POINT('Ctrl Pts',(-46.188816675386,1.09129381988883,-8.40843236441881));
#34918=CARTESIAN_POINT('Ctrl Pts',(-46.2170785613611,1.2996923399296,-8.48604609926933));
#34919=CARTESIAN_POINT('Ctrl Pts',(-46.2240601503759,1.39848091468841,-8.50507279301164));
#34920=CARTESIAN_POINT('Ctrl Pts',(-46.2240601503759,1.5,-8.50507279301164));
#34921=CARTESIAN_POINT('Origin',(-53.2,4.,0.));
#34922=CARTESIAN_POINT('',(-58.,4.,-9.8974744253269));
#34923=CARTESIAN_POINT('',(-58.,4.,-9.8974744253269));
#34924=CARTESIAN_POINT('',(-46.2240601503759,4.,-8.50507279301165));
#34925=CARTESIAN_POINT('Origin',(-53.2,4.,0.));
#34926=CARTESIAN_POINT('',(-46.2240601503759,4.,-8.50507279301165));
#34927=CARTESIAN_POINT('Origin',(59.5,1.5,-1.5));
#34928=CARTESIAN_POINT('',(58.,1.5,-9.8974744253269));
#34929=CARTESIAN_POINT('',(58.,1.5,-46.5));
#34930=CARTESIAN_POINT('',(58.,1.5,-1.5));
#34931=CARTESIAN_POINT('Origin',(59.5,1.5,-46.5));
#34932=CARTESIAN_POINT('Ctrl Pts',(59.5,0.,-7.11055553385247));
#34933=CARTESIAN_POINT('Ctrl Pts',(59.4982621111222,-1.4371403945548E-18,
-7.11441720740794));
#34934=CARTESIAN_POINT('Ctrl Pts',(59.4965230425199,3.02025636478306E-6,
-7.11827835650437));
#34935=CARTESIAN_POINT('Ctrl Pts',(59.2998658346704,0.000687024107904035,
-7.55454952430768));
#34936=CARTESIAN_POINT('Ctrl Pts',(59.0848279111138,0.0390861404145931,
-7.99027457436337));
#34937=CARTESIAN_POINT('Ctrl Pts',(58.6790205873,0.22728069865069,-8.75389357006352));
#34938=CARTESIAN_POINT('Ctrl Pts',(58.5106474320196,0.353869330585278,-9.04860693524623));
#34939=CARTESIAN_POINT('Ctrl Pts',(58.2889293801926,0.60554183624056,-9.42608315641631));
#34940=CARTESIAN_POINT('Ctrl Pts',(58.2055841166437,0.725339698576902,-9.56428617469306));
#34941=CARTESIAN_POINT('Ctrl Pts',(58.0942335303233,0.966223567273979,-9.74614959515892));
#34942=CARTESIAN_POINT('Ctrl Pts',(58.0567637695508,1.07370986494963,-9.80652098494185));
#34943=CARTESIAN_POINT('Ctrl Pts',(58.01124521301,1.29080573116054,-9.87956234691204));
#34944=CARTESIAN_POINT('Ctrl Pts',(58.,1.39399094113258,-9.89747442532689));
#34945=CARTESIAN_POINT('Ctrl Pts',(58.,1.5,-9.89747442532689));
#34946=CARTESIAN_POINT('Origin',(53.2,1.5,0.));
#34947=CARTESIAN_POINT('',(46.2240601503759,1.5,-8.50507279301165));
#34948=CARTESIAN_POINT('Ctrl Pts',(45.209022556391,0.,-5.13753632549022));
#34949=CARTESIAN_POINT('Ctrl Pts',(45.2101706901698,-1.40306831936872E-18,
-5.14245954784354));
#34950=CARTESIAN_POINT('Ctrl Pts',(45.2113202904362,2.87874308709708E-6,
-5.14738243736251));
#34951=CARTESIAN_POINT('Ctrl Pts',(45.3805806079222,0.000852747691324604,
-5.87122802515958));
#34952=CARTESIAN_POINT('Ctrl Pts',(45.5407068115586,0.0644575553358579,
-6.42770683840794));
#34953=CARTESIAN_POINT('Ctrl Pts',(45.799289602191,0.26267602833871,-7.27728490933226));
#34954=CARTESIAN_POINT('Ctrl Pts',(45.9058399421765,0.391768785578204,-7.59761029794919));
#34955=CARTESIAN_POINT('Ctrl Pts',(46.0437392091658,0.637700968927248,-8.00108322240403));
#34956=CARTESIAN_POINT('Ctrl Pts',(46.095986299131,0.754435257863832,-8.14964878644437));
#34957=CARTESIAN_POINT('Ctrl Pts',(46.165500553065,0.98791895592338,-8.34412682404562));
#34958=CARTESIAN_POINT('Ctrl Pts',(46.188816675386,1.09129381988883,-8.40843236441881));
#34959=CARTESIAN_POINT('Ctrl Pts',(46.2170785613611,1.29969233992958,-8.48604609926932));
#34960=CARTESIAN_POINT('Ctrl Pts',(46.2240601503759,1.39848091468841,-8.50507279301164));
#34961=CARTESIAN_POINT('Ctrl Pts',(46.2240601503759,1.5,-8.50507279301164));
#34962=CARTESIAN_POINT('Origin',(53.2,1.5,0.));
#34963=CARTESIAN_POINT('Origin',(0.,1.5,0.));
#34964=CARTESIAN_POINT('',(35.2875682471136,1.5,-31.0449275599944));
#34965=CARTESIAN_POINT('Ctrl Pts',(35.2875682471136,1.5,-31.0449275599943));
#34966=CARTESIAN_POINT('Ctrl Pts',(35.2875682471136,1.35551696906072,-31.0449275599943));
#34967=CARTESIAN_POINT('Ctrl Pts',(35.2589883222484,1.2141695497589,-31.0458481634946));
#34968=CARTESIAN_POINT('Ctrl Pts',(35.1446849201549,0.928422041321496,-31.04943124825));
#34969=CARTESIAN_POINT('Ctrl Pts',(35.0542336624389,0.791102236957392,-31.0522277771702));
#34970=CARTESIAN_POINT('Ctrl Pts',(34.8006041636678,0.513035438790074,-31.0596930143797));
#34971=CARTESIAN_POINT('Ctrl Pts',(34.6252458975058,0.385154103985321,-31.0646128476165));
#34972=CARTESIAN_POINT('Ctrl Pts',(34.2551775861873,0.190507175290631,-31.0741165440007));
#34973=CARTESIAN_POINT('Ctrl Pts',(34.0599327360632,0.120411269801612,-31.0787526147422));
#34974=CARTESIAN_POINT('Ctrl Pts',(33.6525355816955,0.0247093974685881,
-31.0874603040868));
#34975=CARTESIAN_POINT('Ctrl Pts',(33.4376681173913,0.000552123420203993,
-31.0915518418999));
#34976=CARTESIAN_POINT('Ctrl Pts',(33.2214448410094,3.11914488445421E-6,
-31.0951291138549));
#34977=CARTESIAN_POINT('Ctrl Pts',(33.2189876968878,1.08143054073223E-19,
-31.0951696964714));
#34978=CARTESIAN_POINT('Ctrl Pts',(33.2165305534069,0.,-31.0952102098472));
#34979=CARTESIAN_POINT('Origin',(0.,1.5,0.));
#34980=CARTESIAN_POINT('Origin',(36.,1.5,-46.5));
#34981=CARTESIAN_POINT('',(36.,1.5,-68.5));
#34982=CARTESIAN_POINT('Origin',(36.,1.5,-70.));
#34983=CARTESIAN_POINT('Origin',(36.,1.5,-46.5));
#34984=CARTESIAN_POINT('Origin',(18.,1.5,-70.));
#34985=CARTESIAN_POINT('',(-36.,1.5,-68.5));
#34986=CARTESIAN_POINT('Origin',(-36.,1.5,-70.));
#34987=CARTESIAN_POINT('',(18.,1.5,-68.5));
#34988=CARTESIAN_POINT('Origin',(-36.,1.5,-46.5));
#34989=CARTESIAN_POINT('',(-58.,1.5,-46.5));
#34990=CARTESIAN_POINT('Origin',(-59.5,1.5,-46.5));
#34991=CARTESIAN_POINT('Origin',(-36.,1.5,-46.5));
#34992=CARTESIAN_POINT('Origin',(-59.5,1.5,-31.5));
#34993=CARTESIAN_POINT('',(-58.,1.5,-31.5));
#34994=CARTESIAN_POINT('Origin',(-58.,0.,-46.5));
#34995=CARTESIAN_POINT('',(-58.,4.,-46.5));
#34996=CARTESIAN_POINT('',(-58.,0.,-46.5));
#34997=CARTESIAN_POINT('',(-58.,4.,13.5));
#34998=CARTESIAN_POINT('Origin',(-36.,0.,-46.5));
#34999=CARTESIAN_POINT('',(-36.,4.,-68.5));
#35000=CARTESIAN_POINT('',(-36.,0.,-68.5));
#35001=CARTESIAN_POINT('Origin',(-36.,4.,-46.5));
#35002=CARTESIAN_POINT('Origin',(36.,0.,-68.5));
#35003=CARTESIAN_POINT('',(36.,4.,-68.5));
#35004=CARTESIAN_POINT('',(36.,0.,-68.5));
#35005=CARTESIAN_POINT('',(-36.,4.,-68.5));
#35006=CARTESIAN_POINT('Origin',(36.,0.,-46.5));
#35007=CARTESIAN_POINT('',(58.,4.,-46.5));
#35008=CARTESIAN_POINT('',(58.,0.,-46.5));
#35009=CARTESIAN_POINT('Origin',(36.,4.,-46.5));
#35010=CARTESIAN_POINT('Origin',(58.,0.,13.5));
#35011=CARTESIAN_POINT('',(58.,4.,-9.8974744253269));
#35012=CARTESIAN_POINT('',(58.,4.,-9.8974744253269));
#35013=CARTESIAN_POINT('',(58.,4.,-46.5));
#35014=CARTESIAN_POINT('Origin',(53.2,4.,0.));
#35015=CARTESIAN_POINT('',(46.2240601503759,4.,-8.50507279301165));
#35016=CARTESIAN_POINT('',(46.2240601503759,4.,-8.50507279301165));
#35017=CARTESIAN_POINT('Origin',(53.2,4.,0.));
#35018=CARTESIAN_POINT('Origin',(0.,4.,0.));
#35019=CARTESIAN_POINT('',(35.2875682471136,4.,-31.0449275599944));
#35020=CARTESIAN_POINT('',(35.2875682471136,4.,-31.0449275599944));
#35021=CARTESIAN_POINT('Origin',(0.,4.,0.));
#35022=CARTESIAN_POINT('Origin',(-64.5,1.5,-32.5));
#35023=CARTESIAN_POINT('',(-66.,1.5,15.5));
#35024=CARTESIAN_POINT('Origin',(-64.5,1.5,15.5));
#35025=CARTESIAN_POINT('',(-66.,1.5,-48.5));
#35026=CARTESIAN_POINT('',(-66.,1.5,-32.5));
#35027=CARTESIAN_POINT('Origin',(-64.5,1.5,-48.5));
#35028=CARTESIAN_POINT('Origin',(-38.,1.5,-48.5));
#35029=CARTESIAN_POINT('',(-38.,1.5,-76.5));
#35030=CARTESIAN_POINT('Origin',(-38.,1.5,-75.));
#35031=CARTESIAN_POINT('Origin',(-38.,1.5,-48.5));
#35032=CARTESIAN_POINT('Origin',(19.,1.5,-75.));
#35033=CARTESIAN_POINT('',(38.,1.5,-76.5));
#35034=CARTESIAN_POINT('Origin',(38.,1.5,-75.));
#35035=CARTESIAN_POINT('',(19.,1.5,-76.5));
#35036=CARTESIAN_POINT('Origin',(38.,1.5,-48.5));
#35037=CARTESIAN_POINT('',(66.,1.5,-48.5));
#35038=CARTESIAN_POINT('Origin',(64.5,1.5,-48.5));
#35039=CARTESIAN_POINT('Origin',(38.,1.5,-48.5));
#35040=CARTESIAN_POINT('Origin',(64.5,1.5,-0.500000000000003));
#35041=CARTESIAN_POINT('',(66.,1.5,15.5));
#35042=CARTESIAN_POINT('Origin',(64.5,1.5,15.5));
#35043=CARTESIAN_POINT('',(66.,1.5,-0.500000000000003));
#35044=CARTESIAN_POINT('Origin',(38.,1.5,15.5));
#35045=CARTESIAN_POINT('',(38.,1.5,43.5));
#35046=CARTESIAN_POINT('Origin',(38.,1.5,42.));
#35047=CARTESIAN_POINT('Origin',(38.,1.5,15.5));
#35048=CARTESIAN_POINT('Origin',(-19.,1.5,42.));
#35049=CARTESIAN_POINT('',(-19.,1.5,43.5));
#35050=CARTESIAN_POINT('Origin',(-38.,1.5,15.5));
#35051=CARTESIAN_POINT('',(-38.,1.5,43.5));
#35052=CARTESIAN_POINT('Origin',(-38.,1.5,42.));
#35053=CARTESIAN_POINT('Origin',(-38.,1.5,15.5));
#35054=CARTESIAN_POINT('Origin',(-19.,1.5,42.));
#35055=CARTESIAN_POINT('',(-19.,1.5,43.5));
#35056=CARTESIAN_POINT('Origin',(38.,0.,-48.5));
#35057=CARTESIAN_POINT('',(38.,16.5,-76.5));
#35058=CARTESIAN_POINT('',(38.,0.,-76.5));
#35059=CARTESIAN_POINT('',(66.,16.5,-48.5));
#35060=CARTESIAN_POINT('Origin',(38.,16.5,-48.5));
#35061=CARTESIAN_POINT('',(66.,0.,-48.5));
#35062=CARTESIAN_POINT('Origin',(38.,0.,-76.5));
#35063=CARTESIAN_POINT('',(-38.,16.5,-76.5));
#35064=CARTESIAN_POINT('',(-38.,0.,-76.5));
#35065=CARTESIAN_POINT('',(19.,16.5,-76.5));
#35066=CARTESIAN_POINT('Origin',(-38.,0.,-48.5));
#35067=CARTESIAN_POINT('',(-66.,16.5,-48.5));
#35068=CARTESIAN_POINT('',(-66.,0.,-48.5));
#35069=CARTESIAN_POINT('Origin',(-38.,16.5,-48.5));
#35070=CARTESIAN_POINT('Origin',(-66.,0.,-48.5));
#35071=CARTESIAN_POINT('',(-66.,16.5,15.5));
#35072=CARTESIAN_POINT('',(-66.,0.,15.5));
#35073=CARTESIAN_POINT('',(-66.,16.5,-32.5));
#35074=CARTESIAN_POINT('Origin',(-38.,0.,15.5));
#35075=CARTESIAN_POINT('',(-38.,16.5,43.5));
#35076=CARTESIAN_POINT('',(-38.,0.,43.5));
#35077=CARTESIAN_POINT('Origin',(-38.,16.5,15.5));
#35078=CARTESIAN_POINT('Origin',(28.5201839509359,1.5,-26.3988636073762));
#35079=CARTESIAN_POINT('',(29.5808441227157,1.5,-25.3382034355964));
#35080=CARTESIAN_POINT('Origin',(48.7903679018718,4.,-44.5477272147525));
#35081=CARTESIAN_POINT('',(29.5808441227157,4.,-25.3382034355964));
#35082=CARTESIAN_POINT('Origin',(18.6206890143242,1.5,-20.7420093578839));
#35083=CARTESIAN_POINT('',(17.5600288425444,1.5,-21.8026695296637));
#35084=CARTESIAN_POINT('Origin',(28.9913780286485,4.,-33.2340187157677));
#35085=CARTESIAN_POINT('',(17.5600288425444,4.,-21.8026695296637));
#35086=CARTESIAN_POINT('Origin',(0.,1.5,0.));
#35087=CARTESIAN_POINT('',(-3.,1.5,-46.9041575982343));
#35088=CARTESIAN_POINT('Origin',(0.,1.5,0.));
#35089=CARTESIAN_POINT('Ctrl Pts',(-1.49999999999999,0.,-45.4752680036083));
#35090=CARTESIAN_POINT('Ctrl Pts',(-1.50176867612921,1.08300178019032E-19,
-45.4769793019272));
#35091=CARTESIAN_POINT('Ctrl Pts',(-1.50353740181665,3.12821524582445E-6,
-45.4786905515984));
#35092=CARTESIAN_POINT('Ctrl Pts',(-1.6589485445968,0.000552890155855249,
-45.6290430115593));
#35093=CARTESIAN_POINT('Ctrl Pts',(-1.81376170731676,0.0247066439280583,
-45.7780704433202));
#35094=CARTESIAN_POINT('Ctrl Pts',(-2.10792859962105,0.120380195566533,
-46.059925664155));
#35095=CARTESIAN_POINT('Ctrl Pts',(-2.24921701551043,0.190439066398323,
-46.1946602843644));
#35096=CARTESIAN_POINT('Ctrl Pts',(-2.51762496582942,0.385035588736779,
-46.4496283712152));
#35097=CARTESIAN_POINT('Ctrl Pts',(-2.64514766490965,0.512937531198891,
-46.5701910337406));
#35098=CARTESIAN_POINT('Ctrl Pts',(-2.82982150540341,0.791053413169234,
-46.7443046032146));
#35099=CARTESIAN_POINT('Ctrl Pts',(-2.89577102625226,0.928389940435116,
-46.8062984441602));
#35100=CARTESIAN_POINT('Ctrl Pts',(-2.97913882256007,1.21416179467569,-46.8845984232444));
#35101=CARTESIAN_POINT('Ctrl Pts',(-3.,1.35551296703019,-46.9041575982343));
#35102=CARTESIAN_POINT('Ctrl Pts',(-3.,1.5,-46.9041575982343));
#35103=CARTESIAN_POINT('Origin',(-20.7420093578839,1.5,-18.6206890143242));
#35104=CARTESIAN_POINT('',(-35.2875682471136,1.5,-31.0449275599944));
#35105=CARTESIAN_POINT('Ctrl Pts',(-33.2165305534069,0.,-31.0952102098472));
#35106=CARTESIAN_POINT('Ctrl Pts',(-33.2190692967299,1.11734401589879E-19,
-31.0951683510534));
#35107=CARTESIAN_POINT('Ctrl Pts',(-33.2216080407998,3.32975363937025E-6,
-31.0951264183426));
#35108=CARTESIAN_POINT('Ctrl Pts',(-33.4374895579293,0.000569671234467164,
-31.0915543966548));
#35109=CARTESIAN_POINT('Ctrl Pts',(-33.6519250591449,0.0246506601297224,
-31.0874717825085));
#35110=CARTESIAN_POINT('Ctrl Pts',(-34.0573511387189,0.119724494999935,
-31.0788092838542));
#35111=CARTESIAN_POINT('Ctrl Pts',(-34.2510845845319,0.18899207660016,-31.0742145020815));
#35112=CARTESIAN_POINT('Ctrl Pts',(-34.6214706148708,0.382511576258843,
-31.0647171688647));
#35113=CARTESIAN_POINT('Ctrl Pts',(-34.7982799030232,0.510857073213111,
-31.0597601262273));
#35114=CARTESIAN_POINT('Ctrl Pts',(-35.0535067624131,0.790024881159229,
-31.0522501584557));
#35115=CARTESIAN_POINT('Ctrl Pts',(-35.1443641805612,0.927714535375577,
-31.0494412598632));
#35116=CARTESIAN_POINT('Ctrl Pts',(-35.2589537310755,1.21399986481142,-31.0458492854634));
#35117=CARTESIAN_POINT('Ctrl Pts',(-35.2875682471136,1.35542940125323,-31.0449275599943));
#35118=CARTESIAN_POINT('Ctrl Pts',(-35.2875682471136,1.5,-31.0449275599943));
#35119=CARTESIAN_POINT('',(-21.8026695296637,1.5,-17.5600288425444));
#35120=CARTESIAN_POINT('Origin',(0.,1.5,0.));
#35121=CARTESIAN_POINT('Origin',(0.,1.5,0.));
#35122=CARTESIAN_POINT('Origin',(0.,4.,0.));
#35123=CARTESIAN_POINT('',(-3.,4.,-46.9041575982343));
#35124=CARTESIAN_POINT('Origin',(0.,4.,0.));
#35125=CARTESIAN_POINT('',(-3.,4.,-46.9041575982343));
#35126=CARTESIAN_POINT('Origin',(-33.2340187157677,4.,-28.9913780286484));
#35127=CARTESIAN_POINT('',(-35.2875682471136,4.,-31.0449275599944));
#35128=CARTESIAN_POINT('',(-35.2875682471136,4.,-31.0449275599944));
#35129=CARTESIAN_POINT('',(-21.8026695296637,4.,-17.5600288425444));
#35130=CARTESIAN_POINT('Origin',(0.,4.,0.));
#35131=CARTESIAN_POINT('Origin',(0.,4.,0.));
#35132=CARTESIAN_POINT('Origin',(38.,16.5,-48.5));
#35133=CARTESIAN_POINT('Origin',(64.5,16.5,-48.5));
#35134=CARTESIAN_POINT('Origin',(38.,16.5,-75.));
#35135=CARTESIAN_POINT('Origin',(19.,16.5,-75.));
#35136=CARTESIAN_POINT('Origin',(-38.,16.5,-75.));
#35137=CARTESIAN_POINT('Origin',(-38.,16.5,-48.5));
#35138=CARTESIAN_POINT('Origin',(-64.5,16.5,-48.5));
#35139=CARTESIAN_POINT('Origin',(-64.5,16.5,-32.5));
#35140=CARTESIAN_POINT('Origin',(-64.5,16.5,15.5));
#35141=CARTESIAN_POINT('Origin',(-38.,16.5,15.5));
#35142=CARTESIAN_POINT('Origin',(-38.,16.5,42.));
#35143=CARTESIAN_POINT('Origin',(-19.,16.5,42.));
#35144=CARTESIAN_POINT('',(38.,16.5,43.5));
#35145=CARTESIAN_POINT('Origin',(38.,16.5,42.));
#35146=CARTESIAN_POINT('',(-19.,16.5,43.5));
#35147=CARTESIAN_POINT('Origin',(38.,16.5,15.5));
#35148=CARTESIAN_POINT('',(66.,16.5,15.5));
#35149=CARTESIAN_POINT('Origin',(64.5,16.5,15.5));
#35150=CARTESIAN_POINT('Origin',(38.,16.5,15.5));
#35151=CARTESIAN_POINT('Origin',(64.5,16.5,-0.500000000000003));
#35152=CARTESIAN_POINT('',(66.,16.5,-0.500000000000003));
#35153=CARTESIAN_POINT('Origin',(0.,-4.5,0.));
#35154=CARTESIAN_POINT('',(9.86076131526265E-31,-4.5,-41.28));
#35155=CARTESIAN_POINT('Origin',(0.,-4.5,0.));
#35156=CARTESIAN_POINT('',(-9.74328993401634E-15,-6.,-39.78));
#35157=CARTESIAN_POINT('Origin',(9.8065271280287E-31,-4.5,-39.78));
#35158=CARTESIAN_POINT('Origin',(0.,-6.,0.));
#35159=CARTESIAN_POINT('Origin',(0.,-2.7,0.));
#35160=CARTESIAN_POINT('Origin',(0.,-1.8,0.));
#35161=CARTESIAN_POINT('Ctrl Pts',(30.8986928114497,0.551098954354967,27.3735124261331));
#35162=CARTESIAN_POINT('Ctrl Pts',(30.8641827118076,0.506664989272846,27.4124667609344));
#35163=CARTESIAN_POINT('Ctrl Pts',(30.8279866393545,0.464974641768682,27.4531744708043));
#35164=CARTESIAN_POINT('Ctrl Pts',(30.65814747972,0.288491142640607,27.6433707222812));
#35165=CARTESIAN_POINT('Ctrl Pts',(30.5070255439578,0.182453844116018,27.810330268993));
#35166=CARTESIAN_POINT('Ctrl Pts',(30.1879066118572,0.0382329615783753,
28.1564350499007));
#35167=CARTESIAN_POINT('Ctrl Pts',(30.0175971548222,3.00801135180405E-15,
28.3380263942472));
#35168=CARTESIAN_POINT('Ctrl Pts',(29.8463073008423,1.11022302462516E-15,
28.5172989692869));
#35169=CARTESIAN_POINT('Ctrl Pts',(-29.8463073008423,1.14491749414469E-15,
28.5172989692869));
#35170=CARTESIAN_POINT('Ctrl Pts',(-30.0635571076826,3.52780524293222E-15,
28.2899245428733));
#35171=CARTESIAN_POINT('Ctrl Pts',(-30.2801233439677,0.0616272685536241,
28.0577630238579));
#35172=CARTESIAN_POINT('Ctrl Pts',(-30.6381675045497,0.272254431305175,
27.665825911273));
#35173=CARTESIAN_POINT('Ctrl Pts',(-30.7814255694024,0.400109864424864,
27.5058814269562));
#35174=CARTESIAN_POINT('Ctrl Pts',(-30.898692811445,0.551098954348924,27.3735124261384));
#35175=CARTESIAN_POINT('Origin',(0.,-1.8,0.));
#35176=CARTESIAN_POINT('Ctrl Pts',(-35.7247978384162,0.551098954354972,
20.6827759114751));
#35177=CARTESIAN_POINT('Ctrl Pts',(-35.7508728501454,0.506664989272856,
20.6377372509662));
#35178=CARTESIAN_POINT('Ctrl Pts',(-35.7780796730643,0.464974641768688,
20.590545492252));
#35179=CARTESIAN_POINT('Ctrl Pts',(-35.9049685855587,0.288491142640602,
20.3693687346412));
#35180=CARTESIAN_POINT('Ctrl Pts',(-36.0157138907406,0.182453844116013,
20.1732850609533));
#35181=CARTESIAN_POINT('Ctrl Pts',(-36.2434429291201,0.0382329615783755,
19.7612597009681));
#35182=CARTESIAN_POINT('Ctrl Pts',(-36.3620181378251,3.00801135180405E-15,
19.5423518496295));
#35183=CARTESIAN_POINT('Ctrl Pts',(-36.4780836837786,1.11022302462516E-15,
19.3232453474888));
#35184=CARTESIAN_POINT('',(-5.05534198688027E-15,-2.7,-41.28));
#35185=CARTESIAN_POINT('Ctrl Pts',(36.4780836837786,1.21430643318376E-15,
19.3232453474888));
#35186=CARTESIAN_POINT('Ctrl Pts',(36.330875796952,2.8116267922611E-15,
19.601141814568));
#35187=CARTESIAN_POINT('Ctrl Pts',(36.1789096837638,0.0616272685536261,
19.8799001436861));
#35188=CARTESIAN_POINT('Ctrl Pts',(35.9199721561489,0.272254431305173,20.3433240079195));
#35189=CARTESIAN_POINT('Ctrl Pts',(35.8134021815952,0.400109864424854,20.5297320327797));
#35190=CARTESIAN_POINT('Ctrl Pts',(35.7247978384197,0.551098954348926,20.682775911469));
#35191=CARTESIAN_POINT('Origin',(0.,-6.,40.78));
#35192=CARTESIAN_POINT('',(-1.75124492278072E-15,-6.,-14.3));
#35193=CARTESIAN_POINT('Origin',(0.,-6.,0.));
#35194=CARTESIAN_POINT('Origin',(-1.5,1.5,-30.25));
#35195=CARTESIAN_POINT('',(-3.,1.5,-30.25));
#35196=CARTESIAN_POINT('Origin',(-3.,4.,-44.));
#35197=CARTESIAN_POINT('',(-3.,4.,-30.25));
#35198=CARTESIAN_POINT('Origin',(30.5,1.5,22.));
#35199=CARTESIAN_POINT('Origin',(0.,-1.8,0.));
#35200=CARTESIAN_POINT('Origin',(0.,-0.3,0.));
#35201=CARTESIAN_POINT('Origin',(30.5,-0.3,22.));
#35202=CARTESIAN_POINT('Origin',(-30.5,1.5,22.));
#35203=CARTESIAN_POINT('Origin',(0.,-1.8,0.));
#35204=CARTESIAN_POINT('Origin',(0.,-0.3,0.));
#35205=CARTESIAN_POINT('Origin',(-30.5,-0.3,22.));
#35206=CARTESIAN_POINT('Origin',(26.05,16.5,-24.75));
#35207=CARTESIAN_POINT('',(24.55,16.5,-33.));
#35208=CARTESIAN_POINT('Origin',(26.05,16.5,-33.));
#35209=CARTESIAN_POINT('',(24.55,16.5,3.00650789190675E-15));
#35210=CARTESIAN_POINT('',(24.55,16.5,-24.75));
#35211=CARTESIAN_POINT('Origin',(26.05,16.5,4.44089209850063E-15));
#35212=CARTESIAN_POINT('Origin',(0.,16.5,0.));
#35213=CARTESIAN_POINT('',(-24.55,16.5,0.));
#35214=CARTESIAN_POINT('Origin',(-26.05,16.5,0.));
#35215=CARTESIAN_POINT('Origin',(0.,16.5,0.));
#35216=CARTESIAN_POINT('Origin',(-26.05,16.5,-8.25));
#35217=CARTESIAN_POINT('',(-24.55,16.5,-33.));
#35218=CARTESIAN_POINT('Origin',(-26.05,16.5,-33.));
#35219=CARTESIAN_POINT('',(-24.55,16.5,-8.25));
#35220=CARTESIAN_POINT('Origin',(0.,16.5,-33.));
#35221=CARTESIAN_POINT('Origin',(0.,16.5,-33.));
#35222=CARTESIAN_POINT('Origin',(0.,18.,0.));
#35223=CARTESIAN_POINT('',(24.55,15.95,3.00650789190675E-15));
#35224=CARTESIAN_POINT('',(24.55,18.,3.00650789190675E-15));
#35225=CARTESIAN_POINT('',(-24.55,15.95,0.));
#35226=CARTESIAN_POINT('Origin',(0.,15.95,0.));
#35227=CARTESIAN_POINT('',(-24.55,18.,0.));
#35228=CARTESIAN_POINT('Origin',(24.55,18.,-33.));
#35229=CARTESIAN_POINT('',(24.55,15.95,-33.));
#35230=CARTESIAN_POINT('',(24.55,18.,-33.));
#35231=CARTESIAN_POINT('',(24.55,15.95,0.));
#35232=CARTESIAN_POINT('Origin',(-20.95,16.5,-24.75));
#35233=CARTESIAN_POINT('',(-22.45,16.5,-33.));
#35234=CARTESIAN_POINT('Origin',(-20.95,16.5,-33.));
#35235=CARTESIAN_POINT('',(-22.45,16.5,0.));
#35236=CARTESIAN_POINT('',(-22.45,16.5,-24.75));
#35237=CARTESIAN_POINT('Origin',(-20.95,16.5,0.));
#35238=CARTESIAN_POINT('Origin',(0.,16.5,0.));
#35239=CARTESIAN_POINT('',(22.45,16.5,2.74933206408581E-15));
#35240=CARTESIAN_POINT('Origin',(20.95,16.5,2.5656350442137E-15));
#35241=CARTESIAN_POINT('Origin',(0.,16.5,0.));
#35242=CARTESIAN_POINT('Origin',(20.95,16.5,-8.25));
#35243=CARTESIAN_POINT('',(22.45,16.5,-33.));
#35244=CARTESIAN_POINT('Origin',(20.95,16.5,-33.));
#35245=CARTESIAN_POINT('',(22.45,16.5,-8.25));
#35246=CARTESIAN_POINT('Origin',(0.,16.5,-33.));
#35247=CARTESIAN_POINT('Origin',(0.,16.5,-33.));
#35248=CARTESIAN_POINT('Origin',(0.,18.,0.));
#35249=CARTESIAN_POINT('',(-22.45,15.95,0.));
#35250=CARTESIAN_POINT('',(-22.45,18.,0.));
#35251=CARTESIAN_POINT('',(22.45,15.95,2.74933206408581E-15));
#35252=CARTESIAN_POINT('Origin',(0.,15.95,0.));
#35253=CARTESIAN_POINT('',(22.45,18.,2.74933206408581E-15));
#35254=CARTESIAN_POINT('Origin',(-22.45,18.,-33.));
#35255=CARTESIAN_POINT('',(-22.45,15.95,-33.));
#35256=CARTESIAN_POINT('',(-22.45,18.,-33.));
#35257=CARTESIAN_POINT('',(-22.45,15.95,-33.));
#35258=CARTESIAN_POINT('Origin',(0.,18.,-33.));
#35259=CARTESIAN_POINT('',(22.45,15.95,-33.));
#35260=CARTESIAN_POINT('',(22.45,18.,-33.));
#35261=CARTESIAN_POINT('Origin',(0.,15.95,-33.));
#35262=CARTESIAN_POINT('Origin',(22.45,18.,0.));
#35263=CARTESIAN_POINT('',(22.45,15.95,0.));
#35264=CARTESIAN_POINT('Origin',(0.,18.,-33.));
#35265=CARTESIAN_POINT('',(-24.55,15.95,-33.));
#35266=CARTESIAN_POINT('',(-24.55,18.,-33.));
#35267=CARTESIAN_POINT('Origin',(0.,15.95,-33.));
#35268=CARTESIAN_POINT('Origin',(-24.55,18.,0.));
#35269=CARTESIAN_POINT('',(-24.55,15.95,-33.));
#35270=CARTESIAN_POINT('Origin',(0.,15.95,-16.5));
#35271=CARTESIAN_POINT('Origin',(30.5,18.,-16.5));
#35272=CARTESIAN_POINT('',(26.49,9.9,-16.5));
#35273=CARTESIAN_POINT('',(26.49,18.,-16.5));
#35274=CARTESIAN_POINT('Origin',(30.5,9.9,-16.5));
#35275=CARTESIAN_POINT('Origin',(30.5,9.9,-16.5));
#35276=CARTESIAN_POINT('Origin',(-30.5,18.,-16.5));
#35277=CARTESIAN_POINT('',(-34.51,9.9,-16.5));
#35278=CARTESIAN_POINT('',(-34.51,18.,-16.5));
#35279=CARTESIAN_POINT('Origin',(-30.5,9.9,-16.5));
#35280=CARTESIAN_POINT('Origin',(-30.5,9.9,-16.5));
#35281=CARTESIAN_POINT('Origin',(0.,-5.5,14.7));
#35282=CARTESIAN_POINT('',(-1.80023079474661E-15,-5.5,-14.7));
#35283=CARTESIAN_POINT('Origin',(0.,-5.5,0.));
#35284=CARTESIAN_POINT('',(-1.75124492278072E-15,-5.5,-14.3));
#35285=CARTESIAN_POINT('Origin',(0.,-5.5,0.));
#35286=CARTESIAN_POINT('Origin',(0.,-4.85,0.));
#35287=CARTESIAN_POINT('',(-1.80023079474661E-15,-4.2,-14.7));
#35288=CARTESIAN_POINT('',(-1.80023079474661E-15,-4.85,-14.7));
#35289=CARTESIAN_POINT('Origin',(0.,-4.2,0.));
#35290=CARTESIAN_POINT('Origin',(0.,-4.2,14.2));
#35291=CARTESIAN_POINT('',(1.75124492278072E-15,-4.2,-14.3));
#35292=CARTESIAN_POINT('Origin',(0.,-4.2,0.));
#35293=CARTESIAN_POINT('Origin',(0.,-2.,0.));
#35294=CARTESIAN_POINT('',(-1.75124492278072E-15,-2.,-14.3));
#35295=CARTESIAN_POINT('Origin',(0.,-2.,0.));
#35296=CARTESIAN_POINT('',(-1.75124492278072E-15,-2.,-14.3));
#35297=CARTESIAN_POINT('Origin',(0.,4.,-16.5));
#35298=CARTESIAN_POINT('Origin',(0.,4.,0.));
#35299=CARTESIAN_POINT('',(30.8017856625229,4.,35.5));
#35300=CARTESIAN_POINT('Origin',(0.,4.,0.));
#35301=CARTESIAN_POINT('',(30.8017856625229,4.,35.5));
#35302=CARTESIAN_POINT('Origin',(-53.2,4.,0.));
#35303=CARTESIAN_POINT('',(-58.,4.,9.8974744253269));
#35304=CARTESIAN_POINT('Origin',(-53.2,4.,0.));
#35305=CARTESIAN_POINT('',(-58.,4.,9.8974744253269));
#35306=CARTESIAN_POINT('Origin',(0.,4.,0.));
#35307=CARTESIAN_POINT('',(-19.,4.,43.5));
#35308=CARTESIAN_POINT('Origin',(-38.,0.,43.5));
#35309=CARTESIAN_POINT('',(38.,0.,43.5));
#35310=CARTESIAN_POINT('Origin',(-58.,0.,-46.5));
#35311=CARTESIAN_POINT('',(-58.,4.,13.5));
#35312=CARTESIAN_POINT('Origin',(-36.,0.,35.5));
#35313=CARTESIAN_POINT('',(36.,4.,35.5));
#35314=CARTESIAN_POINT('Origin',(0.,4.,-16.5));
#35315=CARTESIAN_POINT('Origin',(0.,4.,-16.5));
#35316=CARTESIAN_POINT('Origin',(66.,0.,15.5));
#35317=CARTESIAN_POINT('',(66.,0.,15.5));
#35318=CARTESIAN_POINT('Origin',(38.,0.,15.5));
#35319=CARTESIAN_POINT('',(0.,0.,0.));
#35320=CARTESIAN_POINT('Origin',(39.75,50.9,-16.5));
#35321=CARTESIAN_POINT('',(40.,50.9,-2.45));
#35322=CARTESIAN_POINT('Origin',(40.,50.9,-16.5));
#35323=CARTESIAN_POINT('',(39.5,50.9,-2.95));
#35324=CARTESIAN_POINT('',(39.75,50.9,-2.7));
#35325=CARTESIAN_POINT('Origin',(39.5,50.9,-16.5));
#35326=CARTESIAN_POINT('Origin',(40.,50.9,-16.5));
#35327=CARTESIAN_POINT('',(22.,50.9,-2.95));
#35328=CARTESIAN_POINT('',(40.,50.9,-2.95));
#35329=CARTESIAN_POINT('Origin',(22.,50.9,-16.5));
#35330=CARTESIAN_POINT('Origin',(40.,50.9,-16.5));
#35331=CARTESIAN_POINT('',(40.,50.9,4.5));
#35332=CARTESIAN_POINT('Origin',(40.,50.9,-16.5));
#35333=CARTESIAN_POINT('Origin',(-39.75,50.9,-16.5));
#35334=CARTESIAN_POINT('',(-40.,50.9,-2.45));
#35335=CARTESIAN_POINT('Origin',(-40.,50.9,-16.5));
#35336=CARTESIAN_POINT('',(-39.5,50.9,-2.95));
#35337=CARTESIAN_POINT('',(-39.75,50.9,-2.7));
#35338=CARTESIAN_POINT('Origin',(-39.5,50.9,-16.5));
#35339=CARTESIAN_POINT('Origin',(-40.,50.9,-16.5));
#35340=CARTESIAN_POINT('',(-22.,50.9,-2.95));
#35341=CARTESIAN_POINT('',(-40.,50.9,-2.95));
#35342=CARTESIAN_POINT('Origin',(-22.,50.9,-16.5));
#35343=CARTESIAN_POINT('Origin',(-40.,50.9,-16.5));
#35344=CARTESIAN_POINT('',(-40.,50.9,4.5));
#35345=CARTESIAN_POINT('Origin',(-40.,50.9,-16.5));
#35346=CARTESIAN_POINT('Origin',(39.7,83.2,4.25));
#35347=CARTESIAN_POINT('',(39.7,84.,25.));
#35348=CARTESIAN_POINT('',(40.5,83.2,25.));
#35349=CARTESIAN_POINT('Origin',(39.7,83.2,25.));
#35350=CARTESIAN_POINT('',(40.5,83.2,-58.));
#35351=CARTESIAN_POINT('',(40.5,83.2,4.25));
#35352=CARTESIAN_POINT('',(39.7,84.,-58.));
#35353=CARTESIAN_POINT('Origin',(39.7,83.2,-58.));
#35354=CARTESIAN_POINT('',(39.7,84.,4.25));
#35355=CARTESIAN_POINT('Origin',(30.5,83.2,-58.));
#35356=CARTESIAN_POINT('',(30.5,83.2,-68.));
#35357=CARTESIAN_POINT('',(30.5,84.,-67.2));
#35358=CARTESIAN_POINT('Origin',(30.5,83.2,-67.2));
#35359=CARTESIAN_POINT('Origin',(30.5,84.,-58.));
#35360=CARTESIAN_POINT('Origin',(30.5,83.2,-58.));
#35361=CARTESIAN_POINT('Origin',(15.25,83.2,-67.2));
#35362=CARTESIAN_POINT('',(-30.5,83.2,-68.));
#35363=CARTESIAN_POINT('',(-30.5,84.,-67.2));
#35364=CARTESIAN_POINT('Origin',(-30.5,83.2,-67.2));
#35365=CARTESIAN_POINT('',(15.25,84.,-67.2));
#35366=CARTESIAN_POINT('',(15.25,83.2,-68.));
#35367=CARTESIAN_POINT('Origin',(-30.5,83.2,-58.));
#35368=CARTESIAN_POINT('',(-40.5,83.2,-58.));
#35369=CARTESIAN_POINT('',(-39.7,84.,-58.));
#35370=CARTESIAN_POINT('Origin',(-39.7,83.2,-58.));
#35371=CARTESIAN_POINT('Origin',(-30.5,84.,-58.));
#35372=CARTESIAN_POINT('Origin',(-30.5,83.2,-58.));
#35373=CARTESIAN_POINT('Origin',(-39.7,83.2,-37.25));
#35374=CARTESIAN_POINT('',(-40.5,83.2,25.));
#35375=CARTESIAN_POINT('',(-39.7,84.,25.));
#35376=CARTESIAN_POINT('Origin',(-39.7,83.2,25.));
#35377=CARTESIAN_POINT('',(-39.7,84.,-37.25));
#35378=CARTESIAN_POINT('',(-40.5,83.2,-37.25));
#35379=CARTESIAN_POINT('Origin',(-30.5,83.2,25.));
#35380=CARTESIAN_POINT('',(-30.5,83.2,35.));
#35381=CARTESIAN_POINT('',(-30.5,84.,34.2));
#35382=CARTESIAN_POINT('Origin',(-30.5,83.2,34.2));
#35383=CARTESIAN_POINT('Origin',(-30.5,84.,25.));
#35384=CARTESIAN_POINT('Origin',(-30.5,83.2,25.));
#35385=CARTESIAN_POINT('Origin',(-15.25,83.2,34.2));
#35386=CARTESIAN_POINT('',(30.5,83.2,35.));
#35387=CARTESIAN_POINT('',(30.5,84.,34.2));
#35388=CARTESIAN_POINT('Origin',(30.5,83.2,34.2));
#35389=CARTESIAN_POINT('',(-15.25,84.,34.2));
#35390=CARTESIAN_POINT('',(-15.25,83.2,35.));
#35391=CARTESIAN_POINT('Origin',(30.5,83.2,25.));
#35392=CARTESIAN_POINT('Origin',(30.5,84.,25.));
#35393=CARTESIAN_POINT('Origin',(30.5,83.2,25.));
#35394=CARTESIAN_POINT('Origin',(-30.5,18.,-58.));
#35395=CARTESIAN_POINT('',(-30.5,18.8,-68.));
#35396=CARTESIAN_POINT('',(-30.5,18.,-68.));
#35397=CARTESIAN_POINT('',(-40.5,18.8,-58.));
#35398=CARTESIAN_POINT('Origin',(-30.5,18.8,-58.));
#35399=CARTESIAN_POINT('',(-40.5,18.,-58.));
#35400=CARTESIAN_POINT('Origin',(30.5,18.,-68.));
#35401=CARTESIAN_POINT('',(30.5,18.8,-68.));
#35402=CARTESIAN_POINT('',(30.5,18.,-68.));
#35403=CARTESIAN_POINT('',(15.25,18.8,-68.));
#35404=CARTESIAN_POINT('Origin',(30.5,18.,-58.));
#35405=CARTESIAN_POINT('',(40.5,18.8,-58.));
#35406=CARTESIAN_POINT('',(40.5,18.,-58.));
#35407=CARTESIAN_POINT('Origin',(30.5,18.8,-58.));
#35408=CARTESIAN_POINT('Origin',(40.5,18.,25.));
#35409=CARTESIAN_POINT('',(40.5,18.8,25.));
#35410=CARTESIAN_POINT('',(40.5,18.,25.));
#35411=CARTESIAN_POINT('',(40.5,18.8,4.25));
#35412=CARTESIAN_POINT('',(40.5,50.9,4.5));
#35413=CARTESIAN_POINT('Origin',(40.5,50.9,-16.5));
#35414=CARTESIAN_POINT('Origin',(0.,84.,-16.5));
#35415=CARTESIAN_POINT('',(26.49,84.,-16.5));
#35416=CARTESIAN_POINT('Origin',(30.5,84.,-16.5));
#35417=CARTESIAN_POINT('',(-34.51,84.,-16.5));
#35418=CARTESIAN_POINT('Origin',(-30.5,84.,-16.5));
#35419=CARTESIAN_POINT('',(10.0119928086271,84.,-16.5));
#35420=CARTESIAN_POINT('',(-10.0119928086271,84.,-16.5));
#35421=CARTESIAN_POINT('Origin',(0.,84.,0.));
#35422=CARTESIAN_POINT('Origin',(0.,84.,-33.));
#35423=CARTESIAN_POINT('',(-35.8,84.,-55.));
#35424=CARTESIAN_POINT('Origin',(-30.5,84.,-55.));
#35425=CARTESIAN_POINT('',(25.2,84.,22.));
#35426=CARTESIAN_POINT('Origin',(30.5,84.,22.));
#35427=CARTESIAN_POINT('',(-35.8,84.,22.));
#35428=CARTESIAN_POINT('Origin',(-30.5,84.,22.));
#35429=CARTESIAN_POINT('',(25.2,84.,-55.));
#35430=CARTESIAN_POINT('Origin',(30.5,84.,-55.));
#35431=CARTESIAN_POINT('Origin',(39.7,18.8,4.25));
#35432=CARTESIAN_POINT('',(39.7,18.,-58.));
#35433=CARTESIAN_POINT('Origin',(39.7,18.8,-58.));
#35434=CARTESIAN_POINT('',(39.7,18.,25.));
#35435=CARTESIAN_POINT('Origin',(39.7,18.8,25.));
#35436=CARTESIAN_POINT('',(39.7,18.,4.25));
#35437=CARTESIAN_POINT('Origin',(30.5,18.8,25.));
#35438=CARTESIAN_POINT('',(30.5,18.8,35.));
#35439=CARTESIAN_POINT('',(30.5,18.,34.2));
#35440=CARTESIAN_POINT('Origin',(30.5,18.8,34.2));
#35441=CARTESIAN_POINT('Origin',(30.5,18.,25.));
#35442=CARTESIAN_POINT('Origin',(30.5,18.8,25.));
#35443=CARTESIAN_POINT('Origin',(-15.25,18.8,34.2));
#35444=CARTESIAN_POINT('',(-30.5,18.8,35.));
#35445=CARTESIAN_POINT('',(-30.5,18.,34.2));
#35446=CARTESIAN_POINT('Origin',(-30.5,18.8,34.2));
#35447=CARTESIAN_POINT('',(-15.25,18.,34.2));
#35448=CARTESIAN_POINT('',(-15.25,18.8,35.));
#35449=CARTESIAN_POINT('Origin',(-30.5,18.8,25.));
#35450=CARTESIAN_POINT('',(-40.5,18.8,25.));
#35451=CARTESIAN_POINT('',(-39.7,18.,25.));
#35452=CARTESIAN_POINT('Origin',(-39.7,18.8,25.));
#35453=CARTESIAN_POINT('Origin',(-30.5,18.,25.));
#35454=CARTESIAN_POINT('Origin',(-30.5,18.8,25.));
#35455=CARTESIAN_POINT('Origin',(-39.7,18.8,-37.25));
#35456=CARTESIAN_POINT('',(-39.7,18.,-58.));
#35457=CARTESIAN_POINT('Origin',(-39.7,18.8,-58.));
#35458=CARTESIAN_POINT('',(-39.7,18.,-37.25));
#35459=CARTESIAN_POINT('',(-40.5,18.8,-37.25));
#35460=CARTESIAN_POINT('Origin',(-30.5,18.8,-58.));
#35461=CARTESIAN_POINT('',(-30.5,18.,-67.2));
#35462=CARTESIAN_POINT('Origin',(-30.5,18.8,-67.2));
#35463=CARTESIAN_POINT('Origin',(-30.5,18.,-58.));
#35464=CARTESIAN_POINT('Origin',(15.25,18.8,-67.2));
#35465=CARTESIAN_POINT('',(30.5,18.,-67.2));
#35466=CARTESIAN_POINT('Origin',(30.5,18.8,-67.2));
#35467=CARTESIAN_POINT('',(15.25,18.,-67.2));
#35468=CARTESIAN_POINT('Origin',(30.5,18.8,-58.));
#35469=CARTESIAN_POINT('Origin',(30.5,18.,-58.));
#35470=CARTESIAN_POINT('Origin',(-30.5,18.,25.));
#35471=CARTESIAN_POINT('',(-40.5,18.,25.));
#35472=CARTESIAN_POINT('',(-30.5,18.,35.));
#35473=CARTESIAN_POINT('Origin',(-30.5,18.,35.));
#35474=CARTESIAN_POINT('',(30.5,18.,35.));
#35475=CARTESIAN_POINT('Origin',(30.5,18.,25.));
#35476=CARTESIAN_POINT('Origin',(0.,18.,-16.5));
#35477=CARTESIAN_POINT('',(26.49,18.,-16.5));
#35478=CARTESIAN_POINT('Origin',(30.5,18.,-16.5));
#35479=CARTESIAN_POINT('',(-34.51,18.,-16.5));
#35480=CARTESIAN_POINT('Origin',(-30.5,18.,-16.5));
#35481=CARTESIAN_POINT('',(-10.0119928086271,18.,-16.5));
#35482=CARTESIAN_POINT('',(10.0119928086271,18.,-16.5));
#35483=CARTESIAN_POINT('Origin',(0.,18.,0.));
#35484=CARTESIAN_POINT('Origin',(0.,18.,-33.));
#35485=CARTESIAN_POINT('',(-35.8,18.,-55.));
#35486=CARTESIAN_POINT('Origin',(-30.5,18.,-55.));
#35487=CARTESIAN_POINT('',(25.2,18.,22.));
#35488=CARTESIAN_POINT('Origin',(30.5,18.,22.));
#35489=CARTESIAN_POINT('',(-35.8,18.,22.));
#35490=CARTESIAN_POINT('Origin',(-30.5,18.,22.));
#35491=CARTESIAN_POINT('',(25.2,18.,-55.));
#35492=CARTESIAN_POINT('Origin',(30.5,18.,-55.));
#35493=CARTESIAN_POINT('Origin',(30.5,84.,-16.5));
#35494=CARTESIAN_POINT('',(26.49,75.9,-16.5));
#35495=CARTESIAN_POINT('',(26.49,84.,-16.5));
#35496=CARTESIAN_POINT('Origin',(30.5,75.9,-16.5));
#35497=CARTESIAN_POINT('Origin',(30.5,75.9,-16.5));
#35498=CARTESIAN_POINT('Origin',(-30.5,84.,-16.5));
#35499=CARTESIAN_POINT('',(-34.51,75.9,-16.5));
#35500=CARTESIAN_POINT('',(-34.51,84.,-16.5));
#35501=CARTESIAN_POINT('Origin',(-30.5,75.9,-16.5));
#35502=CARTESIAN_POINT('Origin',(-30.5,75.9,-16.5));
#35503=CARTESIAN_POINT('Origin',(30.5,18.,-16.5));
#35504=CARTESIAN_POINT('',(26.49,26.1,-16.5));
#35505=CARTESIAN_POINT('',(26.49,18.,-16.5));
#35506=CARTESIAN_POINT('Origin',(30.5,26.1,-16.5));
#35507=CARTESIAN_POINT('Origin',(30.5,26.1,-16.5));
#35508=CARTESIAN_POINT('Origin',(-30.5,18.,-16.5));
#35509=CARTESIAN_POINT('',(-34.51,26.1,-16.5));
#35510=CARTESIAN_POINT('',(-34.51,18.,-16.5));
#35511=CARTESIAN_POINT('Origin',(-30.5,26.1,-16.5));
#35512=CARTESIAN_POINT('Origin',(-30.5,26.1,-16.5));
#35513=CARTESIAN_POINT('Origin',(30.5,18.,-55.));
#35514=CARTESIAN_POINT('',(25.2,18.,-55.));
#35515=CARTESIAN_POINT('Origin',(-30.5,18.,22.));
#35516=CARTESIAN_POINT('',(-35.8,18.,22.));
#35517=CARTESIAN_POINT('Origin',(30.5,18.,22.));
#35518=CARTESIAN_POINT('',(25.2,18.,22.));
#35519=CARTESIAN_POINT('Origin',(-30.5,18.,-55.));
#35520=CARTESIAN_POINT('',(-35.8,18.,-55.));
#35521=CARTESIAN_POINT('Origin',(-22.,50.9,-16.5));
#35522=CARTESIAN_POINT('',(-22.,50.9,-8.5));
#35523=CARTESIAN_POINT('Origin',(-22.,50.9,-16.5));
#35524=CARTESIAN_POINT('',(-17.3274348938324,50.9,-8.5));
#35525=CARTESIAN_POINT('',(-22.,50.9,-8.5));
#35526=CARTESIAN_POINT('',(-10.0119928086271,42.9,-16.5));
#35527=CARTESIAN_POINT('Ctrl Pts',(-10.0119928086271,42.9,-16.5));
#35528=CARTESIAN_POINT('Ctrl Pts',(-10.8243823748144,42.9,-16.0070522124563));
#35529=CARTESIAN_POINT('Ctrl Pts',(-11.5907592092305,42.9452825491298,-15.4594449915334));
#35530=CARTESIAN_POINT('Ctrl Pts',(-13.3968422560143,43.2558356261026,-13.965537209318));
#35531=CARTESIAN_POINT('Ctrl Pts',(-14.3590663403517,43.6180540935561,-12.9614726780539));
#35532=CARTESIAN_POINT('Ctrl Pts',(-15.5310939194137,44.6509559696764,-11.4729026436893));
#35533=CARTESIAN_POINT('Ctrl Pts',(-15.8830436339347,45.0733219142187,-10.9773729587387));
#35534=CARTESIAN_POINT('Ctrl Pts',(-16.4643944901793,46.0739061329322,-10.084517906201));
#35535=CARTESIAN_POINT('Ctrl Pts',(-16.6952841581299,46.6528137937707,-9.68893591004821));
#35536=CARTESIAN_POINT('Ctrl Pts',(-17.0124367279563,47.7580666714417,-9.1193277294487));
#35537=CARTESIAN_POINT('Ctrl Pts',(-17.1347583532058,48.3666931400295,-8.88370547669544));
#35538=CARTESIAN_POINT('Ctrl Pts',(-17.2918616244663,49.6341178547131,-8.57389564467795));
#35539=CARTESIAN_POINT('Ctrl Pts',(-17.3274348938324,50.2928891954098,-8.5));
#35540=CARTESIAN_POINT('Ctrl Pts',(-17.3274348938324,50.9,-8.5));
#35541=CARTESIAN_POINT('',(-10.0119928086271,58.9,-16.5));
#35542=CARTESIAN_POINT('Ctrl Pts',(-10.0119928086271,58.9,-16.5));
#35543=CARTESIAN_POINT('Ctrl Pts',(-10.8243823748144,58.9,-16.9929477875437));
#35544=CARTESIAN_POINT('Ctrl Pts',(-11.5907592092305,58.8547174508702,-17.5405550084666));
#35545=CARTESIAN_POINT('Ctrl Pts',(-13.3968422560143,58.5441643738974,-19.034462790682));
#35546=CARTESIAN_POINT('Ctrl Pts',(-14.3590663403517,58.1819459064439,-20.0385273219461));
#35547=CARTESIAN_POINT('Ctrl Pts',(-15.5310939194137,57.1490440303236,-21.5270973563107));
#35548=CARTESIAN_POINT('Ctrl Pts',(-15.8830436339347,56.7266780857813,-22.0226270412612));
#35549=CARTESIAN_POINT('Ctrl Pts',(-16.4643944901793,55.7260938670678,-22.915482093799));
#35550=CARTESIAN_POINT('Ctrl Pts',(-16.6952841581299,55.1471862062293,-23.3110640899518));
#35551=CARTESIAN_POINT('Ctrl Pts',(-17.0124367279563,54.0419333285583,-23.8806722705513));
#35552=CARTESIAN_POINT('Ctrl Pts',(-17.1347583532058,53.4333068599705,-24.1162945233046));
#35553=CARTESIAN_POINT('Ctrl Pts',(-17.2918616244663,52.1658821452869,-24.4261043553221));
#35554=CARTESIAN_POINT('Ctrl Pts',(-17.3274348938324,51.5071108045901,-24.5));
#35555=CARTESIAN_POINT('Ctrl Pts',(-17.3274348938324,50.2928891954098,-24.5));
#35556=CARTESIAN_POINT('Ctrl Pts',(-17.2918616244663,49.6341178547131,-24.4261043553221));
#35557=CARTESIAN_POINT('Ctrl Pts',(-17.1347583532058,48.3666931400295,-24.1162945233046));
#35558=CARTESIAN_POINT('Ctrl Pts',(-17.0124367279563,47.7580666714417,-23.8806722705513));
#35559=CARTESIAN_POINT('Ctrl Pts',(-16.6952841581299,46.6528137937707,-23.3110640899518));
#35560=CARTESIAN_POINT('Ctrl Pts',(-16.4643944901793,46.0739061329322,-22.915482093799));
#35561=CARTESIAN_POINT('Ctrl Pts',(-15.8830436339347,45.0733219142187,-22.0226270412612));
#35562=CARTESIAN_POINT('Ctrl Pts',(-15.5310939194137,44.6509559696764,-21.5270973563107));
#35563=CARTESIAN_POINT('Ctrl Pts',(-14.3590663403517,43.6180540935561,-20.0385273219461));
#35564=CARTESIAN_POINT('Ctrl Pts',(-13.3968422560143,43.2558356261026,-19.034462790682));
#35565=CARTESIAN_POINT('Ctrl Pts',(-11.5907592092305,42.9452825491298,-17.5405550084666));
#35566=CARTESIAN_POINT('Ctrl Pts',(-10.8243823748144,42.9,-16.9929477875437));
#35567=CARTESIAN_POINT('Ctrl Pts',(-10.0119928086271,42.9,-16.5));
#35568=CARTESIAN_POINT('Ctrl Pts',(-17.3274348938324,50.9,-8.5));
#35569=CARTESIAN_POINT('Ctrl Pts',(-17.3274348938324,51.5071108045902,-8.5));
#35570=CARTESIAN_POINT('Ctrl Pts',(-17.2918616244663,52.1658821452869,-8.57389564467795));
#35571=CARTESIAN_POINT('Ctrl Pts',(-17.1347583532058,53.4333068599705,-8.88370547669544));
#35572=CARTESIAN_POINT('Ctrl Pts',(-17.0124367279563,54.0419333285583,-9.1193277294487));
#35573=CARTESIAN_POINT('Ctrl Pts',(-16.6952841581299,55.1471862062293,-9.68893591004821));
#35574=CARTESIAN_POINT('Ctrl Pts',(-16.4643944901793,55.7260938670678,-10.084517906201));
#35575=CARTESIAN_POINT('Ctrl Pts',(-15.8830436339347,56.7266780857813,-10.9773729587387));
#35576=CARTESIAN_POINT('Ctrl Pts',(-15.5310939194137,57.1490440303236,-11.4729026436893));
#35577=CARTESIAN_POINT('Ctrl Pts',(-14.3590663403517,58.1819459064439,-12.9614726780539));
#35578=CARTESIAN_POINT('Ctrl Pts',(-13.3968422560143,58.5441643738974,-13.965537209318));
#35579=CARTESIAN_POINT('Ctrl Pts',(-11.5907592092305,58.8547174508702,-15.4594449915334));
#35580=CARTESIAN_POINT('Ctrl Pts',(-10.8243823748144,58.9,-16.0070522124563));
#35581=CARTESIAN_POINT('Ctrl Pts',(-10.0119928086271,58.9,-16.5));
#35582=CARTESIAN_POINT('Origin',(0.,18.,0.));
#35583=CARTESIAN_POINT('',(-10.0119928086271,18.,-16.5));
#35584=CARTESIAN_POINT('',(10.0119928086271,58.9,-16.5));
#35585=CARTESIAN_POINT('',(10.0119928086271,18.,-16.5));
#35586=CARTESIAN_POINT('',(17.3274348938324,50.9,-8.5));
#35587=CARTESIAN_POINT('Ctrl Pts',(10.0119928086271,58.9,-16.5));
#35588=CARTESIAN_POINT('Ctrl Pts',(10.8243823748144,58.9,-16.0070522124563));
#35589=CARTESIAN_POINT('Ctrl Pts',(11.5907592092305,58.8547174508702,-15.4594449915334));
#35590=CARTESIAN_POINT('Ctrl Pts',(13.3968422560143,58.5441643738974,-13.965537209318));
#35591=CARTESIAN_POINT('Ctrl Pts',(14.3590663403517,58.1819459064439,-12.9614726780539));
#35592=CARTESIAN_POINT('Ctrl Pts',(15.5310939194137,57.1490440303236,-11.4729026436893));
#35593=CARTESIAN_POINT('Ctrl Pts',(15.8830436339347,56.7266780857813,-10.9773729587387));
#35594=CARTESIAN_POINT('Ctrl Pts',(16.4643944901793,55.7260938670678,-10.084517906201));
#35595=CARTESIAN_POINT('Ctrl Pts',(16.6952841581299,55.1471862062293,-9.68893591004821));
#35596=CARTESIAN_POINT('Ctrl Pts',(17.0124367279563,54.0419333285583,-9.1193277294487));
#35597=CARTESIAN_POINT('Ctrl Pts',(17.1347583532058,53.4333068599705,-8.88370547669544));
#35598=CARTESIAN_POINT('Ctrl Pts',(17.2918616244663,52.1658821452869,-8.57389564467795));
#35599=CARTESIAN_POINT('Ctrl Pts',(17.3274348938324,51.5071108045902,-8.5));
#35600=CARTESIAN_POINT('Ctrl Pts',(17.3274348938324,50.9,-8.5));
#35601=CARTESIAN_POINT('',(10.0119928086271,42.9,-16.5));
#35602=CARTESIAN_POINT('Ctrl Pts',(17.3274348938324,50.9,-8.5));
#35603=CARTESIAN_POINT('Ctrl Pts',(17.3274348938324,50.2928891954098,-8.5));
#35604=CARTESIAN_POINT('Ctrl Pts',(17.2918616244663,49.6341178547131,-8.57389564467795));
#35605=CARTESIAN_POINT('Ctrl Pts',(17.1347583532058,48.3666931400295,-8.88370547669544));
#35606=CARTESIAN_POINT('Ctrl Pts',(17.0124367279563,47.7580666714417,-9.1193277294487));
#35607=CARTESIAN_POINT('Ctrl Pts',(16.6952841581299,46.6528137937707,-9.68893591004821));
#35608=CARTESIAN_POINT('Ctrl Pts',(16.4643944901793,46.0739061329322,-10.084517906201));
#35609=CARTESIAN_POINT('Ctrl Pts',(15.8830436339347,45.0733219142187,-10.9773729587387));
#35610=CARTESIAN_POINT('Ctrl Pts',(15.5310939194137,44.6509559696764,-11.4729026436893));
#35611=CARTESIAN_POINT('Ctrl Pts',(14.3590663403517,43.6180540935561,-12.9614726780539));
#35612=CARTESIAN_POINT('Ctrl Pts',(13.3968422560143,43.2558356261026,-13.965537209318));
#35613=CARTESIAN_POINT('Ctrl Pts',(11.5907592092305,42.9452825491298,-15.4594449915334));
#35614=CARTESIAN_POINT('Ctrl Pts',(10.8243823748144,42.9,-16.0070522124563));
#35615=CARTESIAN_POINT('Ctrl Pts',(10.0119928086271,42.9,-16.5));
#35616=CARTESIAN_POINT('',(10.0119928086271,18.,-16.5));
#35617=CARTESIAN_POINT('',(-10.0119928086271,18.,-16.5));
#35618=CARTESIAN_POINT('Origin',(-22.,50.9,-16.5));
#35619=CARTESIAN_POINT('Origin',(-40.5,50.9,-16.5));
#35620=CARTESIAN_POINT('',(-40.5,50.9,4.5));
#35621=CARTESIAN_POINT('Origin',(-40.5,50.9,-16.5));
#35622=CARTESIAN_POINT('',(-40.5,50.9,4.5));
#35623=CARTESIAN_POINT('Origin',(22.,50.9,-16.5));
#35624=CARTESIAN_POINT('',(22.,50.9,-8.5));
#35625=CARTESIAN_POINT('Origin',(22.,50.9,-16.5));
#35626=CARTESIAN_POINT('',(22.,50.9,-8.5));
#35627=CARTESIAN_POINT('Ctrl Pts',(10.0119928086271,42.9,-16.5));
#35628=CARTESIAN_POINT('Ctrl Pts',(10.8243823748144,42.9,-16.9929477875437));
#35629=CARTESIAN_POINT('Ctrl Pts',(11.5907592092305,42.9452825491298,-17.5405550084666));
#35630=CARTESIAN_POINT('Ctrl Pts',(13.3968422560143,43.2558356261026,-19.034462790682));
#35631=CARTESIAN_POINT('Ctrl Pts',(14.3590663403517,43.6180540935561,-20.0385273219461));
#35632=CARTESIAN_POINT('Ctrl Pts',(15.5310939194137,44.6509559696764,-21.5270973563107));
#35633=CARTESIAN_POINT('Ctrl Pts',(15.8830436339347,45.0733219142187,-22.0226270412612));
#35634=CARTESIAN_POINT('Ctrl Pts',(16.4643944901793,46.0739061329322,-22.915482093799));
#35635=CARTESIAN_POINT('Ctrl Pts',(16.6952841581299,46.6528137937707,-23.3110640899518));
#35636=CARTESIAN_POINT('Ctrl Pts',(17.0124367279563,47.7580666714417,-23.8806722705513));
#35637=CARTESIAN_POINT('Ctrl Pts',(17.1347583532058,48.3666931400295,-24.1162945233046));
#35638=CARTESIAN_POINT('Ctrl Pts',(17.2918616244663,49.6341178547131,-24.4261043553221));
#35639=CARTESIAN_POINT('Ctrl Pts',(17.3274348938324,50.2928891954098,-24.5));
#35640=CARTESIAN_POINT('Ctrl Pts',(17.3274348938324,51.5071108045901,-24.5));
#35641=CARTESIAN_POINT('Ctrl Pts',(17.2918616244663,52.1658821452869,-24.4261043553221));
#35642=CARTESIAN_POINT('Ctrl Pts',(17.1347583532058,53.4333068599705,-24.1162945233046));
#35643=CARTESIAN_POINT('Ctrl Pts',(17.0124367279563,54.0419333285583,-23.8806722705513));
#35644=CARTESIAN_POINT('Ctrl Pts',(16.6952841581299,55.1471862062293,-23.3110640899518));
#35645=CARTESIAN_POINT('Ctrl Pts',(16.4643944901793,55.7260938670678,-22.915482093799));
#35646=CARTESIAN_POINT('Ctrl Pts',(15.8830436339347,56.7266780857813,-22.0226270412612));
#35647=CARTESIAN_POINT('Ctrl Pts',(15.5310939194137,57.1490440303236,-21.5270973563107));
#35648=CARTESIAN_POINT('Ctrl Pts',(14.3590663403517,58.1819459064439,-20.0385273219461));
#35649=CARTESIAN_POINT('Ctrl Pts',(13.3968422560143,58.5441643738974,-19.034462790682));
#35650=CARTESIAN_POINT('Ctrl Pts',(11.5907592092305,58.8547174508702,-17.5405550084666));
#35651=CARTESIAN_POINT('Ctrl Pts',(10.8243823748144,58.9,-16.9929477875437));
#35652=CARTESIAN_POINT('Ctrl Pts',(10.0119928086271,58.9,-16.5));
#35653=CARTESIAN_POINT('Origin',(0.,18.,-33.));
#35654=CARTESIAN_POINT('Origin',(22.,50.9,-16.5));
#35655=CARTESIAN_POINT('Origin',(40.5,50.9,-16.5));
#35656=CARTESIAN_POINT('',(40.5,50.9,4.5));
#35657=CARTESIAN_POINT('Origin',(-40.5,18.,-58.));
#35658=CARTESIAN_POINT('',(0.,0.,0.));
#35659=CARTESIAN_POINT('Origin',(0.,105.05,-16.5));
#35660=CARTESIAN_POINT('',(-7.2,104.8,-16.5));
#35661=CARTESIAN_POINT('Origin',(0.,104.8,-16.5));
#35662=CARTESIAN_POINT('',(-7.7,105.3,-16.5));
#35663=CARTESIAN_POINT('',(-7.45,105.05,-16.5));
#35664=CARTESIAN_POINT('Origin',(0.,105.3,-16.5));
#35665=CARTESIAN_POINT('Origin',(0.,105.3,-16.5));
#35666=CARTESIAN_POINT('',(-11.,105.3,-16.5));
#35667=CARTESIAN_POINT('Origin',(0.,105.3,-16.5));
#35668=CARTESIAN_POINT('Origin',(0.,105.7,-16.5));
#35669=CARTESIAN_POINT('',(-7.2,93.7,-16.5));
#35670=CARTESIAN_POINT('',(-7.2,105.7,-16.5));
#35671=CARTESIAN_POINT('Origin',(0.,93.7,-16.5));
#35672=CARTESIAN_POINT('Origin',(-24.8,84.25,-24.75));
#35673=CARTESIAN_POINT('',(-24.55,84.5,0.));
#35674=CARTESIAN_POINT('',(-25.05,84.,0.));
#35675=CARTESIAN_POINT('',(-24.55,84.5,0.));
#35676=CARTESIAN_POINT('',(-25.05,84.,-33.));
#35677=CARTESIAN_POINT('',(-25.05,84.,-24.75));
#35678=CARTESIAN_POINT('',(-24.55,84.5,-33.));
#35679=CARTESIAN_POINT('',(-25.05,84.,-33.));
#35680=CARTESIAN_POINT('',(-24.55,84.5,-24.75));
#35681=CARTESIAN_POINT('Origin',(0.,84.25,0.));
#35682=CARTESIAN_POINT('',(24.55,84.5,3.00650789190675E-15));
#35683=CARTESIAN_POINT('',(25.05,84.,3.06774023186412E-15));
#35684=CARTESIAN_POINT('',(24.55,84.5,3.00650789190675E-15));
#35685=CARTESIAN_POINT('Origin',(0.,84.,0.));
#35686=CARTESIAN_POINT('Origin',(0.,84.5,0.));
#35687=CARTESIAN_POINT('Origin',(24.8,84.25,-8.25));
#35688=CARTESIAN_POINT('',(24.55,84.5,-33.));
#35689=CARTESIAN_POINT('',(25.05,84.,-33.));
#35690=CARTESIAN_POINT('',(24.55,84.5,-33.));
#35691=CARTESIAN_POINT('',(25.05,84.,-8.25));
#35692=CARTESIAN_POINT('',(24.55,84.5,-8.25));
#35693=CARTESIAN_POINT('Origin',(0.,84.25,-33.));
#35694=CARTESIAN_POINT('Origin',(0.,84.,-33.));
#35695=CARTESIAN_POINT('Origin',(0.,84.5,-33.));
#35696=CARTESIAN_POINT('Origin',(0.,84.,0.));
#35697=CARTESIAN_POINT('',(-24.55,86.05,0.));
#35698=CARTESIAN_POINT('',(-24.55,84.,0.));
#35699=CARTESIAN_POINT('',(24.55,86.05,3.00650789190675E-15));
#35700=CARTESIAN_POINT('Origin',(0.,86.05,0.));
#35701=CARTESIAN_POINT('',(24.55,84.,3.00650789190675E-15));
#35702=CARTESIAN_POINT('Origin',(-24.55,84.,-33.));
#35703=CARTESIAN_POINT('',(-24.55,86.05,-33.));
#35704=CARTESIAN_POINT('',(-24.55,84.,-33.));
#35705=CARTESIAN_POINT('',(-24.55,86.05,-33.));
#35706=CARTESIAN_POINT('Origin',(0.,84.,-16.5));
#35707=CARTESIAN_POINT('',(-30.5,84.,-67.5));
#35708=CARTESIAN_POINT('',(-40.,84.,-58.));
#35709=CARTESIAN_POINT('Origin',(-30.5,84.,-58.));
#35710=CARTESIAN_POINT('',(30.5,84.,-67.5));
#35711=CARTESIAN_POINT('',(15.25,84.,-67.5));
#35712=CARTESIAN_POINT('',(40.,84.,-58.));
#35713=CARTESIAN_POINT('Origin',(30.5,84.,-58.));
#35714=CARTESIAN_POINT('',(40.,84.,25.));
#35715=CARTESIAN_POINT('',(40.,84.,4.25));
#35716=CARTESIAN_POINT('',(30.5,84.,34.5));
#35717=CARTESIAN_POINT('Origin',(30.5,84.,25.));
#35718=CARTESIAN_POINT('',(-30.5,84.,34.5));
#35719=CARTESIAN_POINT('',(-15.25,84.,34.5));
#35720=CARTESIAN_POINT('',(-40.,84.,25.));
#35721=CARTESIAN_POINT('Origin',(-30.5,84.,25.));
#35722=CARTESIAN_POINT('',(-40.,84.,-37.25));
#35723=CARTESIAN_POINT('',(-35.8,84.,-55.));
#35724=CARTESIAN_POINT('Origin',(-30.5,84.,-55.));
#35725=CARTESIAN_POINT('',(25.2,84.,22.));
#35726=CARTESIAN_POINT('Origin',(30.5,84.,22.));
#35727=CARTESIAN_POINT('',(-35.8,84.,22.));
#35728=CARTESIAN_POINT('Origin',(-30.5,84.,22.));
#35729=CARTESIAN_POINT('',(25.2,84.,-55.));
#35730=CARTESIAN_POINT('Origin',(30.5,84.,-55.));
#35731=CARTESIAN_POINT('',(-34.51,84.,-16.5));
#35732=CARTESIAN_POINT('Origin',(-30.5,84.,-16.5));
#35733=CARTESIAN_POINT('',(26.49,84.,-16.5));
#35734=CARTESIAN_POINT('Origin',(30.5,84.,-16.5));
#35735=CARTESIAN_POINT('Origin',(22.2,84.25,-24.75));
#35736=CARTESIAN_POINT('',(22.45,84.5,2.74933206408581E-15));
#35737=CARTESIAN_POINT('',(21.95,84.,4.44089209850063E-15));
#35738=CARTESIAN_POINT('',(22.45,84.5,2.74933206408581E-15));
#35739=CARTESIAN_POINT('',(21.95,84.,-33.));
#35740=CARTESIAN_POINT('',(21.95,84.,-24.75));
#35741=CARTESIAN_POINT('',(22.45,84.5,-33.));
#35742=CARTESIAN_POINT('',(21.95,84.,-33.));
#35743=CARTESIAN_POINT('',(22.45,84.5,-24.75));
#35744=CARTESIAN_POINT('Origin',(0.,84.25,0.));
#35745=CARTESIAN_POINT('',(-22.45,84.5,0.));
#35746=CARTESIAN_POINT('',(-21.95,84.,5.37619944825688E-15));
#35747=CARTESIAN_POINT('',(-22.45,84.5,0.));
#35748=CARTESIAN_POINT('Origin',(0.,84.,0.));
#35749=CARTESIAN_POINT('Origin',(0.,84.5,0.));
#35750=CARTESIAN_POINT('Origin',(-22.2,84.25,-8.25));
#35751=CARTESIAN_POINT('',(-22.45,84.5,-33.));
#35752=CARTESIAN_POINT('',(-21.95,84.,-33.));
#35753=CARTESIAN_POINT('',(-22.45,84.5,-33.));
#35754=CARTESIAN_POINT('',(-21.95,84.,-8.25));
#35755=CARTESIAN_POINT('',(-22.45,84.5,-8.25));
#35756=CARTESIAN_POINT('Origin',(0.,84.25,-33.));
#35757=CARTESIAN_POINT('Origin',(0.,84.,-33.));
#35758=CARTESIAN_POINT('Origin',(0.,84.5,-33.));
#35759=CARTESIAN_POINT('Origin',(0.,84.,0.));
#35760=CARTESIAN_POINT('',(22.45,86.05,2.74933206408581E-15));
#35761=CARTESIAN_POINT('',(22.45,84.,2.74933206408581E-15));
#35762=CARTESIAN_POINT('',(-22.45,86.05,0.));
#35763=CARTESIAN_POINT('Origin',(0.,86.05,0.));
#35764=CARTESIAN_POINT('',(-22.45,84.,0.));
#35765=CARTESIAN_POINT('Origin',(22.45,84.,-33.));
#35766=CARTESIAN_POINT('',(22.45,86.05,-33.));
#35767=CARTESIAN_POINT('',(22.45,84.,-33.));
#35768=CARTESIAN_POINT('',(22.45,86.05,0.));
#35769=CARTESIAN_POINT('Origin',(0.,84.,-16.5));
#35770=CARTESIAN_POINT('Origin',(-30.5,105.45,22.));
#35771=CARTESIAN_POINT('',(-39.,105.7,19.0419601084502));
#35772=CARTESIAN_POINT('',(-39.25,105.45,22.));
#35773=CARTESIAN_POINT('Ctrl Pts',(-39.,105.7,19.0419601084503));
#35774=CARTESIAN_POINT('Ctrl Pts',(-39.25,105.45,20.5209800542251));
#35775=CARTESIAN_POINT('Ctrl Pts',(-39.25,105.45,22.));
#35776=CARTESIAN_POINT('',(-39.,105.2,22.));
#35777=CARTESIAN_POINT('',(-39.25,105.45,22.));
#35778=CARTESIAN_POINT('Origin',(-30.5,105.2,22.));
#35779=CARTESIAN_POINT('',(-39.,105.7,24.9580398915498));
#35780=CARTESIAN_POINT('Ctrl Pts',(-39.25,105.45,22.));
#35781=CARTESIAN_POINT('Ctrl Pts',(-39.25,105.45,23.4790199457749));
#35782=CARTESIAN_POINT('Ctrl Pts',(-39.,105.7,24.9580398915497));
#35783=CARTESIAN_POINT('Origin',(-30.5,105.7,22.));
#35784=CARTESIAN_POINT('Origin',(-39.75,104.95,-37.25));
#35785=CARTESIAN_POINT('',(-39.,105.7,-52.0419601084502));
#35786=CARTESIAN_POINT('',(-39.,105.7,-37.25));
#35787=CARTESIAN_POINT('',(-39.25,105.45,-55.));
#35788=CARTESIAN_POINT('Ctrl Pts',(-39.25,105.45,-55.));
#35789=CARTESIAN_POINT('Ctrl Pts',(-39.25,105.45,-53.5209800542251));
#35790=CARTESIAN_POINT('Ctrl Pts',(-39.,105.7,-52.0419601084503));
#35791=CARTESIAN_POINT('',(-39.,105.7,-57.9580398915498));
#35792=CARTESIAN_POINT('Ctrl Pts',(-39.,105.7,-57.9580398915497));
#35793=CARTESIAN_POINT('Ctrl Pts',(-39.25,105.45,-56.4790199457749));
#35794=CARTESIAN_POINT('Ctrl Pts',(-39.25,105.45,-55.));
#35795=CARTESIAN_POINT('',(-39.,105.7,-58.));
#35796=CARTESIAN_POINT('',(-39.,105.7,-37.25));
#35797=CARTESIAN_POINT('',(-40.1464466094067,104.553553390593,-58.));
#35798=CARTESIAN_POINT('',(-40.5,104.2,-58.));
#35799=CARTESIAN_POINT('',(-40.1464466094067,104.553553390593,25.));
#35800=CARTESIAN_POINT('',(-40.1464466094067,104.553553390593,-47.625));
#35801=CARTESIAN_POINT('',(-39.,105.7,25.));
#35802=CARTESIAN_POINT('',(-40.5,104.2,25.));
#35803=CARTESIAN_POINT('',(-39.,105.7,-37.25));
#35804=CARTESIAN_POINT('Origin',(-30.5,105.7,22.));
#35805=CARTESIAN_POINT('',(-39.,93.7,22.));
#35806=CARTESIAN_POINT('',(-39.,105.7,22.));
#35807=CARTESIAN_POINT('Origin',(-30.5,93.7,22.));
#35808=CARTESIAN_POINT('Origin',(-30.5,105.45,-55.));
#35809=CARTESIAN_POINT('',(-39.,105.2,-55.));
#35810=CARTESIAN_POINT('',(-39.25,105.45,-55.));
#35811=CARTESIAN_POINT('Origin',(-30.5,105.2,-55.));
#35812=CARTESIAN_POINT('Origin',(-30.5,105.7,-55.));
#35813=CARTESIAN_POINT('Origin',(-30.5,105.7,-55.));
#35814=CARTESIAN_POINT('',(-39.,93.7,-55.));
#35815=CARTESIAN_POINT('',(-39.,105.7,-55.));
#35816=CARTESIAN_POINT('Origin',(-30.5,93.7,-55.));
#35817=CARTESIAN_POINT('Origin',(30.5,105.45,-55.));
#35818=CARTESIAN_POINT('',(39.,105.7,-52.0419601084502));
#35819=CARTESIAN_POINT('',(39.25,105.45,-55.));
#35820=CARTESIAN_POINT('Ctrl Pts',(39.,105.7,-52.0419601084503));
#35821=CARTESIAN_POINT('Ctrl Pts',(39.25,105.45,-53.5209800542251));
#35822=CARTESIAN_POINT('Ctrl Pts',(39.25,105.45,-55.));
#35823=CARTESIAN_POINT('',(39.,105.2,-55.));
#35824=CARTESIAN_POINT('',(39.25,105.45,-55.));
#35825=CARTESIAN_POINT('',(22.,105.2,-55.));
#35826=CARTESIAN_POINT('Origin',(30.5,105.2,-55.));
#35827=CARTESIAN_POINT('Origin',(30.5,105.2,-55.));
#35828=CARTESIAN_POINT('',(39.,105.7,-57.9580398915498));
#35829=CARTESIAN_POINT('Ctrl Pts',(39.25,105.45,-55.));
#35830=CARTESIAN_POINT('Ctrl Pts',(39.25,105.45,-56.4790199457749));
#35831=CARTESIAN_POINT('Ctrl Pts',(39.,105.7,-57.9580398915497));
#35832=CARTESIAN_POINT('Origin',(30.5,105.7,-55.));
#35833=CARTESIAN_POINT('Origin',(39.75,104.95,4.25));
#35834=CARTESIAN_POINT('',(39.,105.7,19.0419601084502));
#35835=CARTESIAN_POINT('',(39.,105.7,4.25));
#35836=CARTESIAN_POINT('',(39.25,105.45,22.));
#35837=CARTESIAN_POINT('Ctrl Pts',(39.25,105.45,22.));
#35838=CARTESIAN_POINT('Ctrl Pts',(39.25,105.45,20.5209800542251));
#35839=CARTESIAN_POINT('Ctrl Pts',(39.,105.7,19.0419601084503));
#35840=CARTESIAN_POINT('',(39.,105.7,24.9580398915498));
#35841=CARTESIAN_POINT('Ctrl Pts',(39.,105.7,24.9580398915497));
#35842=CARTESIAN_POINT('Ctrl Pts',(39.25,105.45,23.4790199457749));
#35843=CARTESIAN_POINT('Ctrl Pts',(39.25,105.45,22.));
#35844=CARTESIAN_POINT('',(39.,105.7,25.));
#35845=CARTESIAN_POINT('',(39.,105.7,4.25));
#35846=CARTESIAN_POINT('',(40.1464466094067,104.553553390593,25.));
#35847=CARTESIAN_POINT('',(39.,105.7,25.));
#35848=CARTESIAN_POINT('',(40.1464466094067,104.553553390593,-58.));
#35849=CARTESIAN_POINT('',(40.1464466094067,104.553553390593,14.625));
#35850=CARTESIAN_POINT('',(39.,105.7,-58.));
#35851=CARTESIAN_POINT('',(40.5,104.2,-58.));
#35852=CARTESIAN_POINT('',(39.,105.7,4.25));
#35853=CARTESIAN_POINT('Origin',(30.5,105.7,-55.));
#35854=CARTESIAN_POINT('',(22.,93.7,-55.));
#35855=CARTESIAN_POINT('',(22.,105.7,-55.));
#35856=CARTESIAN_POINT('Origin',(30.5,93.7,-55.));
#35857=CARTESIAN_POINT('Origin',(30.5,105.45,22.));
#35858=CARTESIAN_POINT('',(39.,105.2,22.));
#35859=CARTESIAN_POINT('',(39.25,105.45,22.));
#35860=CARTESIAN_POINT('',(22.,105.2,22.));
#35861=CARTESIAN_POINT('Origin',(30.5,105.2,22.));
#35862=CARTESIAN_POINT('Origin',(30.5,105.2,22.));
#35863=CARTESIAN_POINT('Origin',(30.5,105.7,22.));
#35864=CARTESIAN_POINT('Origin',(30.5,105.7,22.));
#35865=CARTESIAN_POINT('',(22.,93.7,22.));
#35866=CARTESIAN_POINT('',(22.,105.7,22.));
#35867=CARTESIAN_POINT('Origin',(30.5,93.7,22.));
#35868=CARTESIAN_POINT('Origin',(-30.5,84.25,-58.));
#35869=CARTESIAN_POINT('',(-40.5,84.5,-58.));
#35870=CARTESIAN_POINT('',(-40.,84.,-58.));
#35871=CARTESIAN_POINT('',(-30.5,84.5,-68.));
#35872=CARTESIAN_POINT('Origin',(-30.5,84.5,-58.));
#35873=CARTESIAN_POINT('',(-30.5,84.5,-68.));
#35874=CARTESIAN_POINT('Origin',(-40.25,84.25,-37.25));
#35875=CARTESIAN_POINT('',(-40.5,84.5,25.));
#35876=CARTESIAN_POINT('',(-40.,84.,25.));
#35877=CARTESIAN_POINT('',(-40.5,84.5,-37.25));
#35878=CARTESIAN_POINT('Origin',(-30.5,84.25,25.));
#35879=CARTESIAN_POINT('',(-30.5,84.5,35.));
#35880=CARTESIAN_POINT('',(-30.5,84.,34.5));
#35881=CARTESIAN_POINT('Origin',(-30.5,84.5,25.));
#35882=CARTESIAN_POINT('Origin',(-15.25,84.25,34.75));
#35883=CARTESIAN_POINT('',(30.5,84.5,35.));
#35884=CARTESIAN_POINT('',(30.5,84.,34.5));
#35885=CARTESIAN_POINT('',(-15.25,84.5,35.));
#35886=CARTESIAN_POINT('Origin',(30.5,84.25,25.));
#35887=CARTESIAN_POINT('',(40.5,84.5,25.));
#35888=CARTESIAN_POINT('',(40.,84.,25.));
#35889=CARTESIAN_POINT('Origin',(30.5,84.5,25.));
#35890=CARTESIAN_POINT('Origin',(40.25,84.25,4.25));
#35891=CARTESIAN_POINT('',(40.5,84.5,-58.));
#35892=CARTESIAN_POINT('',(40.,84.,-58.));
#35893=CARTESIAN_POINT('',(40.5,84.5,4.25));
#35894=CARTESIAN_POINT('Origin',(30.5,84.25,-58.));
#35895=CARTESIAN_POINT('',(30.5,84.5,-68.));
#35896=CARTESIAN_POINT('',(30.5,84.,-67.5));
#35897=CARTESIAN_POINT('Origin',(30.5,84.5,-58.));
#35898=CARTESIAN_POINT('Origin',(15.25,84.25,-67.75));
#35899=CARTESIAN_POINT('',(15.25,84.5,-68.));
#35900=CARTESIAN_POINT('Origin',(40.5,84.,25.));
#35901=CARTESIAN_POINT('',(40.5,103.7,-58.));
#35902=CARTESIAN_POINT('',(40.5,84.,-58.));
#35903=CARTESIAN_POINT('',(40.5,103.7,25.));
#35904=CARTESIAN_POINT('',(40.5,103.7,14.625));
#35905=CARTESIAN_POINT('',(40.5,84.,25.));
#35906=CARTESIAN_POINT('Origin',(30.5,84.,-58.));
#35907=CARTESIAN_POINT('',(30.5,103.7,-68.));
#35908=CARTESIAN_POINT('',(30.5,84.,-68.));
#35909=CARTESIAN_POINT('Origin',(30.5,103.7,-58.));
#35910=CARTESIAN_POINT('Origin',(30.5,84.,-68.));
#35911=CARTESIAN_POINT('',(-30.5,103.7,-68.));
#35912=CARTESIAN_POINT('',(-30.5,84.,-68.));
#35913=CARTESIAN_POINT('',(22.875,103.7,-68.));
#35914=CARTESIAN_POINT('Origin',(-30.5,84.,-58.));
#35915=CARTESIAN_POINT('',(-40.5,103.7,-58.));
#35916=CARTESIAN_POINT('',(-40.5,84.,-58.));
#35917=CARTESIAN_POINT('Origin',(-30.5,103.7,-58.));
#35918=CARTESIAN_POINT('Origin',(40.3232233047034,104.126776695297,14.625));
#35919=CARTESIAN_POINT('',(40.5,103.7,-58.));
#35920=CARTESIAN_POINT('',(40.1464466094067,104.553553390593,25.));
#35921=CARTESIAN_POINT('Origin',(30.5,104.126776695297,-58.));
#35922=CARTESIAN_POINT('',(30.5,104.553553390593,-67.6464466094067));
#35923=CARTESIAN_POINT('',(30.5,103.7,-68.));
#35924=CARTESIAN_POINT('Origin',(30.5,104.553553390593,-58.));
#35925=CARTESIAN_POINT('Origin',(22.875,104.126776695297,-67.8232233047034));
#35926=CARTESIAN_POINT('',(-30.5,104.553553390593,-67.6464466094067));
#35927=CARTESIAN_POINT('',(-30.5,103.7,-68.));
#35928=CARTESIAN_POINT('',(22.875,104.553553390593,-67.6464466094067));
#35929=CARTESIAN_POINT('Origin',(-30.5,104.126776695297,-58.));
#35930=CARTESIAN_POINT('',(-40.5,103.7,-58.));
#35931=CARTESIAN_POINT('Origin',(-30.5,104.553553390593,-58.));
#35932=CARTESIAN_POINT('Origin',(-40.3232233047034,104.126776695297,-47.625));
#35933=CARTESIAN_POINT('',(-40.5,103.7,25.));
#35934=CARTESIAN_POINT('',(-40.5,103.7,25.));
#35935=CARTESIAN_POINT('',(-40.5,103.7,-47.625));
#35936=CARTESIAN_POINT('Origin',(-30.5,104.126776695297,25.));
#35937=CARTESIAN_POINT('',(-30.5,103.7,35.));
#35938=CARTESIAN_POINT('',(-30.5,104.553553390593,34.6464466094067));
#35939=CARTESIAN_POINT('',(-30.5,103.7,35.));
#35940=CARTESIAN_POINT('Origin',(-30.5,104.553553390593,25.));
#35941=CARTESIAN_POINT('Origin',(-30.5,103.7,25.));
#35942=CARTESIAN_POINT('Origin',(-22.875,104.126776695297,34.8232233047034));
#35943=CARTESIAN_POINT('',(30.5,103.7,35.));
#35944=CARTESIAN_POINT('',(30.5,104.553553390593,34.6464466094067));
#35945=CARTESIAN_POINT('',(30.5,103.7,35.));
#35946=CARTESIAN_POINT('',(-22.875,104.553553390593,34.6464466094067));
#35947=CARTESIAN_POINT('',(-22.875,103.7,35.));
#35948=CARTESIAN_POINT('Origin',(30.5,104.126776695297,25.));
#35949=CARTESIAN_POINT('Origin',(30.5,104.553553390593,25.));
#35950=CARTESIAN_POINT('Origin',(30.5,103.7,25.));
#35951=CARTESIAN_POINT('Origin',(-30.5,104.95,25.));
#35952=CARTESIAN_POINT('',(-30.5,105.7,33.5));
#35953=CARTESIAN_POINT('',(-30.5,104.2,35.));
#35954=CARTESIAN_POINT('Origin',(-30.5,105.7,25.));
#35955=CARTESIAN_POINT('Origin',(-15.25,104.95,34.25));
#35956=CARTESIAN_POINT('',(30.5,105.7,33.5));
#35957=CARTESIAN_POINT('',(30.5,104.2,35.));
#35958=CARTESIAN_POINT('',(-15.25,105.7,33.5));
#35959=CARTESIAN_POINT('Origin',(30.5,104.95,25.));
#35960=CARTESIAN_POINT('Origin',(30.5,105.7,25.));
#35961=CARTESIAN_POINT('Origin',(30.5,104.95,-58.));
#35962=CARTESIAN_POINT('',(30.5,105.7,-66.5));
#35963=CARTESIAN_POINT('',(30.5,104.2,-68.));
#35964=CARTESIAN_POINT('Origin',(30.5,105.7,-58.));
#35965=CARTESIAN_POINT('Origin',(15.25,104.95,-67.25));
#35966=CARTESIAN_POINT('',(-30.5,105.7,-66.5));
#35967=CARTESIAN_POINT('',(-30.5,104.2,-68.));
#35968=CARTESIAN_POINT('',(15.25,105.7,-66.5));
#35969=CARTESIAN_POINT('Origin',(-30.5,104.95,-58.));
#35970=CARTESIAN_POINT('Origin',(-30.5,105.7,-58.));
#35971=CARTESIAN_POINT('Origin',(0.,105.7,-16.5));
#35972=CARTESIAN_POINT('',(-11.,105.7,-16.5));
#35973=CARTESIAN_POINT('Origin',(0.,105.7,-16.5));
#35974=CARTESIAN_POINT('Origin',(0.,84.,-33.));
#35975=CARTESIAN_POINT('',(-22.45,86.05,-33.));
#35976=CARTESIAN_POINT('',(-22.45,84.,-33.));
#35977=CARTESIAN_POINT('Origin',(0.,86.05,-33.));
#35978=CARTESIAN_POINT('Origin',(-22.45,84.,0.));
#35979=CARTESIAN_POINT('',(-22.45,86.05,-33.));
#35980=CARTESIAN_POINT('Origin',(0.,84.,-33.));
#35981=CARTESIAN_POINT('',(24.55,86.05,-33.));
#35982=CARTESIAN_POINT('',(24.55,84.,-33.));
#35983=CARTESIAN_POINT('Origin',(0.,86.05,-33.));
#35984=CARTESIAN_POINT('Origin',(24.55,84.,0.));
#35985=CARTESIAN_POINT('',(24.55,86.05,0.));
#35986=CARTESIAN_POINT('Origin',(0.,86.05,-16.5));
#35987=CARTESIAN_POINT('Origin',(0.,105.7,-16.5));
#35988=CARTESIAN_POINT('',(-11.,105.7,-16.5));
#35989=CARTESIAN_POINT('Origin',(0.,93.7,-16.5));
#35990=CARTESIAN_POINT('Origin',(30.5,84.,-16.5));
#35991=CARTESIAN_POINT('',(26.49,92.1,-16.5));
#35992=CARTESIAN_POINT('',(26.49,84.,-16.5));
#35993=CARTESIAN_POINT('Origin',(30.5,92.1,-16.5));
#35994=CARTESIAN_POINT('Origin',(30.5,92.1,-16.5));
#35995=CARTESIAN_POINT('Origin',(-30.5,84.,-16.5));
#35996=CARTESIAN_POINT('',(-34.51,92.1,-16.5));
#35997=CARTESIAN_POINT('',(-34.51,84.,-16.5));
#35998=CARTESIAN_POINT('Origin',(-30.5,92.1,-16.5));
#35999=CARTESIAN_POINT('Origin',(-30.5,92.1,-16.5));
#36000=CARTESIAN_POINT('Origin',(30.5,93.7,-55.));
#36001=CARTESIAN_POINT('',(25.2,93.7,-55.));
#36002=CARTESIAN_POINT('Origin',(30.5,93.7,-55.));
#36003=CARTESIAN_POINT('',(25.2,93.7,-55.));
#36004=CARTESIAN_POINT('Origin',(-30.5,93.7,22.));
#36005=CARTESIAN_POINT('',(-35.8,93.7,22.));
#36006=CARTESIAN_POINT('Origin',(-30.5,93.7,22.));
#36007=CARTESIAN_POINT('',(-35.8,93.7,22.));
#36008=CARTESIAN_POINT('Origin',(30.5,93.7,22.));
#36009=CARTESIAN_POINT('',(25.2,93.7,22.));
#36010=CARTESIAN_POINT('Origin',(30.5,93.7,22.));
#36011=CARTESIAN_POINT('',(25.2,93.7,22.));
#36012=CARTESIAN_POINT('Origin',(-30.5,93.7,-55.));
#36013=CARTESIAN_POINT('',(-35.8,93.7,-55.));
#36014=CARTESIAN_POINT('Origin',(-30.5,93.7,-55.));
#36015=CARTESIAN_POINT('',(-35.8,93.7,-55.));
#36016=CARTESIAN_POINT('Origin',(30.5,93.7,-55.));
#36017=CARTESIAN_POINT('Origin',(-30.5,93.7,22.));
#36018=CARTESIAN_POINT('Origin',(30.5,93.7,22.));
#36019=CARTESIAN_POINT('Origin',(-30.5,93.7,-55.));
#36020=CARTESIAN_POINT('Origin',(30.5,84.,25.));
#36021=CARTESIAN_POINT('',(30.5,84.,35.));
#36022=CARTESIAN_POINT('Origin',(-30.5,84.,35.));
#36023=CARTESIAN_POINT('',(-30.5,84.,35.));
#36024=CARTESIAN_POINT('Origin',(-30.5,84.,25.));
#36025=CARTESIAN_POINT('',(-40.5,84.,25.));
#36026=CARTESIAN_POINT('Origin',(-40.5,84.,-58.));
#36027=CARTESIAN_POINT('',(0.,0.,0.));
#36028=CARTESIAN_POINT('Origin',(-4.52295818048544,37.28,-5.95914969938874));
#36029=CARTESIAN_POINT('',(-9.89112836854344,37.2481324154382,-12.6120676561534));
#36030=CARTESIAN_POINT('',(-10.0197923273836,37.03,-13.1160858846074));
#36031=CARTESIAN_POINT('',(-9.14322579460993,38.5161005118286,-9.68229203158593));
#36032=CARTESIAN_POINT('',(-7.86882139091927,37.03,-10.47057043093));
#36033=CARTESIAN_POINT('',(-4.32898314662489,37.03,-6.11686363738662));
#36034=CARTESIAN_POINT('',(-8.24055326038937,37.53,-10.1351955192135));
#36035=CARTESIAN_POINT('',(-8.10824010307448,37.3520314584495,-10.2545678870352));
#36036=CARTESIAN_POINT('',(-9.43386642869197,37.53,-11.6028715227817));
#36037=CARTESIAN_POINT('',(-4.71693321434598,37.53,-5.80143576139086));
#36038=CARTESIAN_POINT('',(-9.69653989065522,37.4321844925501,-12.0809901437375));
#36039=CARTESIAN_POINT('',(-7.88714667228405,38.1059743550985,-8.78752995225675));
#36040=CARTESIAN_POINT('',(-8.64161158510598,38.4299914950389,-9.20184382239172));
#36041=CARTESIAN_POINT('Origin',(0.,37.03,0.));
#36042=CARTESIAN_POINT('',(-9.23658232924928,37.03,-9.23658232924928));
#36043=CARTESIAN_POINT('',(-9.23658232924928,37.03,-9.23658232924928));
#36044=CARTESIAN_POINT('',(-10.0358241714444,37.03,-13.1788877890042));
#36045=CARTESIAN_POINT('',(-9.89112836854344,37.03,-12.6120676561534));
#36046=CARTESIAN_POINT('',(-10.1356594341564,37.03,-13.7749103120746));
#36047=CARTESIAN_POINT('',(-10.0358241714444,37.03,-13.1788877890042));
#36048=CARTESIAN_POINT('',(-10.192780409838,37.03,-14.3959225765489));
#36049=CARTESIAN_POINT('',(-10.1356594341564,37.03,-13.7749103120746));
#36050=CARTESIAN_POINT('',(-10.208136822609,37.03,-15.0386712143394));
#36051=CARTESIAN_POINT('',(-10.192780409838,37.03,-14.3959225765489));
#36052=CARTESIAN_POINT('',(-10.1820769523934,37.03,-15.7003835976467));
#36053=CARTESIAN_POINT('',(-10.208136822609,37.03,-15.0386712143394));
#36054=CARTESIAN_POINT('',(-10.1146191541229,37.03,-16.3785524197668));
#36055=CARTESIAN_POINT('',(-10.1820769523934,37.03,-15.7003835976467));
#36056=CARTESIAN_POINT('',(-9.87089260802487,37.03,-16.5265840124582));
#36057=CARTESIAN_POINT('',(-10.1146191541229,37.03,-16.3785524197668));
#36058=CARTESIAN_POINT('',(-9.62500000000001,37.03,-16.6709890228504));
#36059=CARTESIAN_POINT('',(-9.87089260802487,37.03,-16.5265840124582));
#36060=CARTESIAN_POINT('',(-9.37699528855417,37.03,-16.8117357628067));
#36061=CARTESIAN_POINT('',(-9.62500000000001,37.03,-16.6709890228504));
#36062=CARTESIAN_POINT('',(-9.12693289567173,37.03,-16.9487933469585));
#36063=CARTESIAN_POINT('',(-9.37699528855417,37.03,-16.8117357628067));
#36064=CARTESIAN_POINT('',(-8.50589256852587,37.03,-16.6681291028841));
#36065=CARTESIAN_POINT('',(-9.12693289567173,37.03,-16.9487933469585));
#36066=CARTESIAN_POINT('',(-7.91980289947518,37.03,-16.3598414208564));
#36067=CARTESIAN_POINT('',(-8.50589256852587,37.03,-16.6681291028841));
#36068=CARTESIAN_POINT('',(-7.37084445728623,37.03,-16.0251680583905));
#36069=CARTESIAN_POINT('',(-7.91980289947518,37.03,-16.3598414208564));
#36070=CARTESIAN_POINT('',(-6.86159254803069,37.03,-15.6651937101241));
#36071=CARTESIAN_POINT('',(-7.37084445728623,37.03,-16.0251680583905));
#36072=CARTESIAN_POINT('',(-6.39533953317998,37.03,-15.2807225748869));
#36073=CARTESIAN_POINT('',(-6.86159254803069,37.03,-15.6651937101241));
#36074=CARTESIAN_POINT('',(-6.34896741059669,37.03,-15.2354376384622));
#36075=CARTESIAN_POINT('',(-6.39533953317998,37.03,-15.2807225748869));
#36076=CARTESIAN_POINT('',(-5.13336928983992,37.03,-12.0498844378435));
#36077=CARTESIAN_POINT('',(-2.79567366841787,37.03,-5.92380243612285));
#36078=CARTESIAN_POINT('',(-3.38082377665168,37.03,-12.617406105901));
#36079=CARTESIAN_POINT('',(-4.65706016176646,37.03,-12.2041262243426));
#36080=CARTESIAN_POINT('',(-1.57931400691349,37.03,-13.0021906807592));
#36081=CARTESIAN_POINT('',(-3.38082377665168,37.03,-12.617406105901));
#36082=CARTESIAN_POINT('',(-2.11935175385489,37.03,-16.3687597379803));
#36083=CARTESIAN_POINT('',(-0.690577558838534,37.03,-7.46185087477454));
#36084=CARTESIAN_POINT('',(-2.10183478588267,37.03,-16.4311637046244));
#36085=CARTESIAN_POINT('',(-2.25993461117485,37.03,-15.8679351687486));
#36086=CARTESIAN_POINT('',(-1.8902833980495,37.03,-16.997251982187));
#36087=CARTESIAN_POINT('',(-2.10183478588267,37.03,-16.4311637046244));
#36088=CARTESIAN_POINT('',(-1.62924548184168,37.03,-17.5636248671243));
#36089=CARTESIAN_POINT('',(-1.8902833980495,37.03,-16.997251982187));
#36090=CARTESIAN_POINT('',(-1.32117020651705,37.03,-18.1279397220842));
#36091=CARTESIAN_POINT('',(-1.62924548184168,37.03,-17.5636248671243));
#36092=CARTESIAN_POINT('',(-0.967745505237382,37.03,-18.6879695209193));
#36093=CARTESIAN_POINT('',(-1.32117020651705,37.03,-18.1279397220842));
#36094=CARTESIAN_POINT('',(-0.57024092719168,37.03,-19.2415520497946));
#36095=CARTESIAN_POINT('',(-0.967745505237382,37.03,-18.6879695209193));
#36096=CARTESIAN_POINT('',(-0.285151750348432,37.03,-19.247887896579));
#36097=CARTESIAN_POINT('',(-0.57024092719168,37.03,-19.2415520497946));
#36098=CARTESIAN_POINT('',(1.17872254417933E-15,37.03,-19.25));
#36099=CARTESIAN_POINT('',(-0.285151750348432,37.03,-19.247887896579));
#36100=CARTESIAN_POINT('',(0.285151750348434,37.03,-19.247887896579));
#36101=CARTESIAN_POINT('',(1.17872254417933E-15,37.03,-19.25));
#36102=CARTESIAN_POINT('',(0.570240927191682,37.03,-19.2415520497946));
#36103=CARTESIAN_POINT('',(0.285151750348434,37.03,-19.247887896579));
#36104=CARTESIAN_POINT('',(0.967745505237385,37.03,-18.6879695209193));
#36105=CARTESIAN_POINT('',(0.570240927191682,37.03,-19.2415520497946));
#36106=CARTESIAN_POINT('',(1.32117020651705,37.03,-18.1279397220842));
#36107=CARTESIAN_POINT('',(0.967745505237385,37.03,-18.6879695209193));
#36108=CARTESIAN_POINT('',(1.62924548184168,37.03,-17.5636248671243));
#36109=CARTESIAN_POINT('',(1.32117020651705,37.03,-18.1279397220842));
#36110=CARTESIAN_POINT('',(1.8902833980495,37.03,-16.997251982187));
#36111=CARTESIAN_POINT('',(1.62924548184168,37.03,-17.5636248671243));
#36112=CARTESIAN_POINT('',(2.10183478588268,37.03,-16.4311637046244));
#36113=CARTESIAN_POINT('',(1.8902833980495,37.03,-16.997251982187));
#36114=CARTESIAN_POINT('',(2.11935175385489,37.03,-16.3687597379803));
#36115=CARTESIAN_POINT('',(2.10183478588268,37.03,-16.4311637046244));
#36116=CARTESIAN_POINT('',(1.57931400691349,37.03,-13.0021906807592));
#36117=CARTESIAN_POINT('',(0.540776800520309,37.03,-6.52800023089146));
#36118=CARTESIAN_POINT('',(3.38082377665168,37.03,-12.617406105901));
#36119=CARTESIAN_POINT('',(2.0689307051291,37.03,-12.8976134221558));
#36120=CARTESIAN_POINT('',(5.13336928983992,37.03,-12.0498844378435));
#36121=CARTESIAN_POINT('',(3.38082377665168,37.03,-12.617406105901));
#36122=CARTESIAN_POINT('',(6.34896741059669,37.03,-15.2354376384623));
#36123=CARTESIAN_POINT('',(3.13286772814966,37.03,-6.80744119622516));
#36124=CARTESIAN_POINT('',(6.39533953317997,37.03,-15.2807225748869));
#36125=CARTESIAN_POINT('',(5.97680680020517,37.03,-14.8720022673282));
#36126=CARTESIAN_POINT('',(6.86159254803069,37.03,-15.6651937101241));
#36127=CARTESIAN_POINT('',(6.39533953317997,37.03,-15.2807225748869));
#36128=CARTESIAN_POINT('',(7.37084445728622,37.03,-16.0251680583905));
#36129=CARTESIAN_POINT('',(6.86159254803069,37.03,-15.6651937101241));
#36130=CARTESIAN_POINT('',(7.91980289947518,37.03,-16.3598414208564));
#36131=CARTESIAN_POINT('',(7.37084445728622,37.03,-16.0251680583905));
#36132=CARTESIAN_POINT('',(8.50589256852587,37.03,-16.6681291028841));
#36133=CARTESIAN_POINT('',(7.91980289947518,37.03,-16.3598414208564));
#36134=CARTESIAN_POINT('',(9.12693289567173,37.03,-16.9487933469585));
#36135=CARTESIAN_POINT('',(8.50589256852587,37.03,-16.6681291028841));
#36136=CARTESIAN_POINT('',(9.37699528855417,37.03,-16.8117357628067));
#36137=CARTESIAN_POINT('',(9.12693289567173,37.03,-16.9487933469585));
#36138=CARTESIAN_POINT('',(9.625,37.03,-16.6709890228504));
#36139=CARTESIAN_POINT('',(9.37699528855417,37.03,-16.8117357628067));
#36140=CARTESIAN_POINT('',(9.87089260802485,37.03,-16.5265840124582));
#36141=CARTESIAN_POINT('',(9.625,37.03,-16.6709890228504));
#36142=CARTESIAN_POINT('',(10.1146191541229,37.03,-16.3785524197668));
#36143=CARTESIAN_POINT('',(9.87089260802485,37.03,-16.5265840124582));
#36144=CARTESIAN_POINT('',(10.1820769523934,37.03,-15.7003835976467));
#36145=CARTESIAN_POINT('',(10.1146191541229,37.03,-16.3785524197668));
#36146=CARTESIAN_POINT('',(10.208136822609,37.03,-15.0386712143394));
#36147=CARTESIAN_POINT('',(10.1820769523934,37.03,-15.7003835976467));
#36148=CARTESIAN_POINT('',(10.192780409838,37.03,-14.3959225765489));
#36149=CARTESIAN_POINT('',(10.208136822609,37.03,-15.0386712143394));
#36150=CARTESIAN_POINT('',(10.1356594341564,37.03,-13.7749103120746));
#36151=CARTESIAN_POINT('',(10.192780409838,37.03,-14.3959225765489));
#36152=CARTESIAN_POINT('',(10.0358241714444,37.03,-13.1788877890042));
#36153=CARTESIAN_POINT('',(10.1356594341564,37.03,-13.7749103120746));
#36154=CARTESIAN_POINT('',(10.0197923273836,37.03,-13.1160858846074));
#36155=CARTESIAN_POINT('',(10.0358241714444,37.03,-13.1788877890042));
#36156=CARTESIAN_POINT('',(7.86882139091926,37.03,-10.47057043093));
#36157=CARTESIAN_POINT('',(3.73232656247359,37.03,-5.38302563560254));
#36158=CARTESIAN_POINT('',(9.23658232924928,37.03,-9.23658232924928));
#36159=CARTESIAN_POINT('',(8.24055326038937,37.03,-10.1351955192135));
#36160=CARTESIAN_POINT('',(10.47057043093,37.03,-7.86882139091926));
#36161=CARTESIAN_POINT('',(9.23658232924928,37.03,-9.23658232924928));
#36162=CARTESIAN_POINT('',(13.1160858846074,37.03,-10.0197923273836));
#36163=CARTESIAN_POINT('',(6.11686363738662,37.03,-4.32898314662489));
#36164=CARTESIAN_POINT('',(13.1788877890042,37.03,-10.0358241714444));
#36165=CARTESIAN_POINT('',(12.6120676561534,37.03,-9.89112836854343));
#36166=CARTESIAN_POINT('',(13.7749103120746,37.03,-10.1356594341564));
#36167=CARTESIAN_POINT('',(13.1788877890042,37.03,-10.0358241714444));
#36168=CARTESIAN_POINT('',(14.3959225765489,37.03,-10.192780409838));
#36169=CARTESIAN_POINT('',(13.7749103120746,37.03,-10.1356594341564));
#36170=CARTESIAN_POINT('',(15.0386712143394,37.03,-10.208136822609));
#36171=CARTESIAN_POINT('',(14.3959225765489,37.03,-10.192780409838));
#36172=CARTESIAN_POINT('',(15.7003835976467,37.03,-10.1820769523934));
#36173=CARTESIAN_POINT('',(15.0386712143394,37.03,-10.208136822609));
#36174=CARTESIAN_POINT('',(16.3785524197668,37.03,-10.1146191541229));
#36175=CARTESIAN_POINT('',(15.7003835976467,37.03,-10.1820769523934));
#36176=CARTESIAN_POINT('',(16.5265840124582,37.03,-9.87089260802485));
#36177=CARTESIAN_POINT('',(16.3785524197668,37.03,-10.1146191541229));
#36178=CARTESIAN_POINT('',(16.6709890228504,37.03,-9.625));
#36179=CARTESIAN_POINT('',(16.5265840124582,37.03,-9.87089260802485));
#36180=CARTESIAN_POINT('',(16.8117357628067,37.03,-9.37699528855417));
#36181=CARTESIAN_POINT('',(16.6709890228504,37.03,-9.625));
#36182=CARTESIAN_POINT('',(16.9487933469585,37.03,-9.12693289567172));
#36183=CARTESIAN_POINT('',(16.8117357628067,37.03,-9.37699528855417));
#36184=CARTESIAN_POINT('',(16.6681291028841,37.03,-8.50589256852586));
#36185=CARTESIAN_POINT('',(16.9487933469585,37.03,-9.12693289567172));
#36186=CARTESIAN_POINT('',(16.3598414208564,37.03,-7.91980289947517));
#36187=CARTESIAN_POINT('',(16.6681291028841,37.03,-8.50589256852586));
#36188=CARTESIAN_POINT('',(16.0251680583905,37.03,-7.37084445728621));
#36189=CARTESIAN_POINT('',(16.3598414208564,37.03,-7.91980289947517));
#36190=CARTESIAN_POINT('',(15.6651937101241,37.03,-6.86159254803069));
#36191=CARTESIAN_POINT('',(16.0251680583905,37.03,-7.37084445728621));
#36192=CARTESIAN_POINT('',(15.2807225748869,37.03,-6.39533953317997));
#36193=CARTESIAN_POINT('',(15.6651937101241,37.03,-6.86159254803069));
#36194=CARTESIAN_POINT('',(15.2354376384623,37.03,-6.34896741059669));
#36195=CARTESIAN_POINT('',(15.2807225748869,37.03,-6.39533953317997));
#36196=CARTESIAN_POINT('',(12.0498844378435,37.03,-5.13336928983991));
#36197=CARTESIAN_POINT('',(5.92380243612284,37.03,-2.79567366841787));
#36198=CARTESIAN_POINT('',(12.617406105901,37.03,-3.38082377665168));
#36199=CARTESIAN_POINT('',(12.2041262243426,37.03,-4.65706016176646));
#36200=CARTESIAN_POINT('',(13.0021906807592,37.03,-1.57931400691349));
#36201=CARTESIAN_POINT('',(12.617406105901,37.03,-3.38082377665168));
#36202=CARTESIAN_POINT('',(16.3687597379803,37.03,-2.11935175385489));
#36203=CARTESIAN_POINT('',(7.46185087477454,37.03,-0.690577558838536));
#36204=CARTESIAN_POINT('',(16.4311637046244,37.03,-2.10183478588267));
#36205=CARTESIAN_POINT('',(15.8679351687486,37.03,-2.25993461117485));
#36206=CARTESIAN_POINT('',(16.997251982187,37.03,-1.8902833980495));
#36207=CARTESIAN_POINT('',(16.4311637046244,37.03,-2.10183478588267));
#36208=CARTESIAN_POINT('',(17.5636248671243,37.03,-1.62924548184168));
#36209=CARTESIAN_POINT('',(16.997251982187,37.03,-1.8902833980495));
#36210=CARTESIAN_POINT('',(18.1279397220842,37.03,-1.32117020651705));
#36211=CARTESIAN_POINT('',(17.5636248671243,37.03,-1.62924548184168));
#36212=CARTESIAN_POINT('',(18.6879695209193,37.03,-0.967745505237384));
#36213=CARTESIAN_POINT('',(18.1279397220842,37.03,-1.32117020651705));
#36214=CARTESIAN_POINT('',(19.2415520497946,37.03,-0.570240927191682));
#36215=CARTESIAN_POINT('',(18.6879695209193,37.03,-0.967745505237384));
#36216=CARTESIAN_POINT('',(19.247887896579,37.03,-0.285151750348434));
#36217=CARTESIAN_POINT('',(19.2415520497946,37.03,-0.570240927191682));
#36218=CARTESIAN_POINT('',(19.25,37.03,0.));
#36219=CARTESIAN_POINT('',(19.247887896579,37.03,-0.285151750348434));
#36220=CARTESIAN_POINT('',(19.247887896579,37.03,0.285151750348434));
#36221=CARTESIAN_POINT('',(19.25,37.03,0.));
#36222=CARTESIAN_POINT('',(19.2415520497946,37.03,0.570240927191682));
#36223=CARTESIAN_POINT('',(19.247887896579,37.03,0.285151750348434));
#36224=CARTESIAN_POINT('',(18.6879695209193,37.03,0.967745505237384));
#36225=CARTESIAN_POINT('',(19.2415520497946,37.03,0.570240927191682));
#36226=CARTESIAN_POINT('',(18.1279397220842,37.03,1.32117020651705));
#36227=CARTESIAN_POINT('',(18.6879695209193,37.03,0.967745505237384));
#36228=CARTESIAN_POINT('',(17.5636248671243,37.03,1.62924548184168));
#36229=CARTESIAN_POINT('',(18.1279397220842,37.03,1.32117020651705));
#36230=CARTESIAN_POINT('',(16.997251982187,37.03,1.8902833980495));
#36231=CARTESIAN_POINT('',(17.5636248671243,37.03,1.62924548184168));
#36232=CARTESIAN_POINT('',(16.4311637046244,37.03,2.10183478588267));
#36233=CARTESIAN_POINT('',(16.997251982187,37.03,1.8902833980495));
#36234=CARTESIAN_POINT('',(16.3687597379803,37.03,2.11935175385489));
#36235=CARTESIAN_POINT('',(16.4311637046244,37.03,2.10183478588267));
#36236=CARTESIAN_POINT('',(13.0021906807592,37.03,1.57931400691349));
#36237=CARTESIAN_POINT('',(6.52800023089146,37.03,0.540776800520309));
#36238=CARTESIAN_POINT('',(12.617406105901,37.03,3.38082377665168));
#36239=CARTESIAN_POINT('',(12.8976134221558,37.03,2.0689307051291));
#36240=CARTESIAN_POINT('',(12.0498844378435,37.03,5.13336928983991));
#36241=CARTESIAN_POINT('',(12.617406105901,37.03,3.38082377665168));
#36242=CARTESIAN_POINT('',(15.2354376384623,37.03,6.34896741059669));
#36243=CARTESIAN_POINT('',(6.80744119622516,37.03,3.13286772814966));
#36244=CARTESIAN_POINT('',(15.2807225748869,37.03,6.39533953317997));
#36245=CARTESIAN_POINT('',(14.8720022673282,37.03,5.97680680020517));
#36246=CARTESIAN_POINT('',(15.6651937101241,37.03,6.86159254803069));
#36247=CARTESIAN_POINT('',(15.2807225748869,37.03,6.39533953317997));
#36248=CARTESIAN_POINT('',(16.0251680583905,37.03,7.37084445728621));
#36249=CARTESIAN_POINT('',(15.6651937101241,37.03,6.86159254803069));
#36250=CARTESIAN_POINT('',(16.3598414208564,37.03,7.91980289947517));
#36251=CARTESIAN_POINT('',(16.0251680583905,37.03,7.37084445728621));
#36252=CARTESIAN_POINT('',(16.6681291028841,37.03,8.50589256852586));
#36253=CARTESIAN_POINT('',(16.3598414208564,37.03,7.91980289947517));
#36254=CARTESIAN_POINT('',(16.9487933469585,37.03,9.12693289567172));
#36255=CARTESIAN_POINT('',(16.6681291028841,37.03,8.50589256852586));
#36256=CARTESIAN_POINT('',(16.8117357628067,37.03,9.37699528855417));
#36257=CARTESIAN_POINT('',(16.9487933469585,37.03,9.12693289567172));
#36258=CARTESIAN_POINT('',(16.6709890228504,37.03,9.625));
#36259=CARTESIAN_POINT('',(16.8117357628067,37.03,9.37699528855417));
#36260=CARTESIAN_POINT('',(16.5265840124582,37.03,9.87089260802485));
#36261=CARTESIAN_POINT('',(16.6709890228504,37.03,9.625));
#36262=CARTESIAN_POINT('',(16.3785524197668,37.03,10.1146191541229));
#36263=CARTESIAN_POINT('',(16.5265840124582,37.03,9.87089260802485));
#36264=CARTESIAN_POINT('',(15.7003835976467,37.03,10.1820769523934));
#36265=CARTESIAN_POINT('',(16.3785524197668,37.03,10.1146191541229));
#36266=CARTESIAN_POINT('',(15.0386712143394,37.03,10.208136822609));
#36267=CARTESIAN_POINT('',(15.7003835976467,37.03,10.1820769523934));
#36268=CARTESIAN_POINT('',(14.3959225765489,37.03,10.192780409838));
#36269=CARTESIAN_POINT('',(15.0386712143394,37.03,10.208136822609));
#36270=CARTESIAN_POINT('',(13.7749103120746,37.03,10.1356594341564));
#36271=CARTESIAN_POINT('',(14.3959225765489,37.03,10.192780409838));
#36272=CARTESIAN_POINT('',(13.1788877890042,37.03,10.0358241714444));
#36273=CARTESIAN_POINT('',(13.7749103120746,37.03,10.1356594341564));
#36274=CARTESIAN_POINT('',(13.1160858846074,37.03,10.0197923273836));
#36275=CARTESIAN_POINT('',(13.1788877890042,37.03,10.0358241714444));
#36276=CARTESIAN_POINT('',(10.47057043093,37.03,7.86882139091926));
#36277=CARTESIAN_POINT('',(5.38302563560253,37.03,3.73232656247359));
#36278=CARTESIAN_POINT('',(9.23658232924928,37.03,9.23658232924928));
#36279=CARTESIAN_POINT('',(10.1351955192135,37.03,8.24055326038936));
#36280=CARTESIAN_POINT('',(7.86882139091926,37.03,10.47057043093));
#36281=CARTESIAN_POINT('',(9.23658232924928,37.03,9.23658232924928));
#36282=CARTESIAN_POINT('',(10.0197923273836,37.03,13.1160858846074));
#36283=CARTESIAN_POINT('',(4.32898314662489,37.03,6.11686363738663));
#36284=CARTESIAN_POINT('',(10.0358241714444,37.03,13.1788877890042));
#36285=CARTESIAN_POINT('',(9.89112836854343,37.03,12.6120676561534));
#36286=CARTESIAN_POINT('',(10.1356594341564,37.03,13.7749103120746));
#36287=CARTESIAN_POINT('',(10.0358241714444,37.03,13.1788877890042));
#36288=CARTESIAN_POINT('',(10.192780409838,37.03,14.3959225765489));
#36289=CARTESIAN_POINT('',(10.1356594341564,37.03,13.7749103120746));
#36290=CARTESIAN_POINT('',(10.208136822609,37.03,15.0386712143394));
#36291=CARTESIAN_POINT('',(10.192780409838,37.03,14.3959225765489));
#36292=CARTESIAN_POINT('',(10.1820769523934,37.03,15.7003835976467));
#36293=CARTESIAN_POINT('',(10.208136822609,37.03,15.0386712143394));
#36294=CARTESIAN_POINT('',(10.1146191541229,37.03,16.3785524197668));
#36295=CARTESIAN_POINT('',(10.1820769523934,37.03,15.7003835976467));
#36296=CARTESIAN_POINT('',(9.87089260802485,37.03,16.5265840124582));
#36297=CARTESIAN_POINT('',(10.1146191541229,37.03,16.3785524197668));
#36298=CARTESIAN_POINT('',(9.625,37.03,16.6709890228504));
#36299=CARTESIAN_POINT('',(9.87089260802485,37.03,16.5265840124582));
#36300=CARTESIAN_POINT('',(9.37699528855417,37.03,16.8117357628067));
#36301=CARTESIAN_POINT('',(9.625,37.03,16.6709890228504));
#36302=CARTESIAN_POINT('',(9.12693289567173,37.03,16.9487933469585));
#36303=CARTESIAN_POINT('',(9.37699528855417,37.03,16.8117357628067));
#36304=CARTESIAN_POINT('',(8.50589256852587,37.03,16.6681291028841));
#36305=CARTESIAN_POINT('',(9.12693289567173,37.03,16.9487933469585));
#36306=CARTESIAN_POINT('',(7.91980289947518,37.03,16.3598414208564));
#36307=CARTESIAN_POINT('',(8.50589256852587,37.03,16.6681291028841));
#36308=CARTESIAN_POINT('',(7.37084445728622,37.03,16.0251680583905));
#36309=CARTESIAN_POINT('',(7.91980289947518,37.03,16.3598414208564));
#36310=CARTESIAN_POINT('',(6.86159254803069,37.03,15.6651937101241));
#36311=CARTESIAN_POINT('',(7.37084445728622,37.03,16.0251680583905));
#36312=CARTESIAN_POINT('',(6.39533953317997,37.03,15.2807225748869));
#36313=CARTESIAN_POINT('',(6.86159254803069,37.03,15.6651937101241));
#36314=CARTESIAN_POINT('',(6.34896741059669,37.03,15.2354376384623));
#36315=CARTESIAN_POINT('',(6.39533953317997,37.03,15.2807225748869));
#36316=CARTESIAN_POINT('',(5.13336928983992,37.03,12.0498844378435));
#36317=CARTESIAN_POINT('',(2.79567366841787,37.03,5.92380243612285));
#36318=CARTESIAN_POINT('',(3.38082377665168,37.03,12.617406105901));
#36319=CARTESIAN_POINT('',(4.65706016176646,37.03,12.2041262243426));
#36320=CARTESIAN_POINT('',(1.57931400691349,37.03,13.0021906807592));
#36321=CARTESIAN_POINT('',(3.38082377665168,37.03,12.617406105901));
#36322=CARTESIAN_POINT('',(2.11935175385489,37.03,16.3687597379803));
#36323=CARTESIAN_POINT('',(0.690577558838536,37.03,7.46185087477454));
#36324=CARTESIAN_POINT('',(2.10183478588268,37.03,16.4311637046244));
#36325=CARTESIAN_POINT('',(2.25993461117485,37.03,15.8679351687486));
#36326=CARTESIAN_POINT('',(1.8902833980495,37.03,16.997251982187));
#36327=CARTESIAN_POINT('',(2.10183478588268,37.03,16.4311637046244));
#36328=CARTESIAN_POINT('',(1.62924548184168,37.03,17.5636248671243));
#36329=CARTESIAN_POINT('',(1.8902833980495,37.03,16.997251982187));
#36330=CARTESIAN_POINT('',(1.32117020651705,37.03,18.1279397220842));
#36331=CARTESIAN_POINT('',(1.62924548184168,37.03,17.5636248671243));
#36332=CARTESIAN_POINT('',(0.967745505237385,37.03,18.6879695209193));
#36333=CARTESIAN_POINT('',(1.32117020651705,37.03,18.1279397220842));
#36334=CARTESIAN_POINT('',(0.570240927191682,37.03,19.2415520497946));
#36335=CARTESIAN_POINT('',(0.967745505237385,37.03,18.6879695209193));
#36336=CARTESIAN_POINT('',(0.285151750348434,37.03,19.247887896579));
#36337=CARTESIAN_POINT('',(0.570240927191682,37.03,19.2415520497946));
#36338=CARTESIAN_POINT('',(1.17872254417933E-15,37.03,19.25));
#36339=CARTESIAN_POINT('',(0.285151750348434,37.03,19.247887896579));
#36340=CARTESIAN_POINT('',(-0.285151750348432,37.03,19.247887896579));
#36341=CARTESIAN_POINT('',(1.17872254417933E-15,37.03,19.25));
#36342=CARTESIAN_POINT('',(-0.57024092719168,37.03,19.2415520497946));
#36343=CARTESIAN_POINT('',(-0.285151750348432,37.03,19.247887896579));
#36344=CARTESIAN_POINT('',(-0.967745505237382,37.03,18.6879695209193));
#36345=CARTESIAN_POINT('',(-0.57024092719168,37.03,19.2415520497946));
#36346=CARTESIAN_POINT('',(-1.32117020651705,37.03,18.1279397220842));
#36347=CARTESIAN_POINT('',(-0.967745505237382,37.03,18.6879695209193));
#36348=CARTESIAN_POINT('',(-1.62924548184168,37.03,17.5636248671243));
#36349=CARTESIAN_POINT('',(-1.32117020651705,37.03,18.1279397220842));
#36350=CARTESIAN_POINT('',(-1.8902833980495,37.03,16.997251982187));
#36351=CARTESIAN_POINT('',(-1.62924548184168,37.03,17.5636248671243));
#36352=CARTESIAN_POINT('',(-2.10183478588267,37.03,16.4311637046244));
#36353=CARTESIAN_POINT('',(-1.8902833980495,37.03,16.997251982187));
#36354=CARTESIAN_POINT('',(-2.11935175385489,37.03,16.3687597379803));
#36355=CARTESIAN_POINT('',(-2.10183478588267,37.03,16.4311637046244));
#36356=CARTESIAN_POINT('',(-1.57931400691349,37.03,13.0021906807592));
#36357=CARTESIAN_POINT('',(-0.540776800520307,37.03,6.52800023089147));
#36358=CARTESIAN_POINT('',(-3.38082377665168,37.03,12.617406105901));
#36359=CARTESIAN_POINT('',(-2.0689307051291,37.03,12.8976134221558));
#36360=CARTESIAN_POINT('',(-5.13336928983991,37.03,12.0498844378435));
#36361=CARTESIAN_POINT('',(-3.38082377665168,37.03,12.617406105901));
#36362=CARTESIAN_POINT('',(-6.34896741059669,37.03,15.2354376384623));
#36363=CARTESIAN_POINT('',(-3.13286772814965,37.03,6.80744119622516));
#36364=CARTESIAN_POINT('',(-6.39533953317997,37.03,15.2807225748869));
#36365=CARTESIAN_POINT('',(-5.97680680020517,37.03,14.8720022673282));
#36366=CARTESIAN_POINT('',(-6.86159254803068,37.03,15.6651937101241));
#36367=CARTESIAN_POINT('',(-6.39533953317997,37.03,15.2807225748869));
#36368=CARTESIAN_POINT('',(-7.37084445728621,37.03,16.0251680583905));
#36369=CARTESIAN_POINT('',(-6.86159254803068,37.03,15.6651937101241));
#36370=CARTESIAN_POINT('',(-7.91980289947517,37.03,16.3598414208564));
#36371=CARTESIAN_POINT('',(-7.37084445728621,37.03,16.0251680583905));
#36372=CARTESIAN_POINT('',(-8.50589256852586,37.03,16.6681291028841));
#36373=CARTESIAN_POINT('',(-7.91980289947517,37.03,16.3598414208564));
#36374=CARTESIAN_POINT('',(-9.12693289567172,37.03,16.9487933469585));
#36375=CARTESIAN_POINT('',(-8.50589256852586,37.03,16.6681291028841));
#36376=CARTESIAN_POINT('',(-9.37699528855417,37.03,16.8117357628067));
#36377=CARTESIAN_POINT('',(-9.12693289567172,37.03,16.9487933469585));
#36378=CARTESIAN_POINT('',(-9.625,37.03,16.6709890228504));
#36379=CARTESIAN_POINT('',(-9.37699528855417,37.03,16.8117357628067));
#36380=CARTESIAN_POINT('',(-9.87089260802485,37.03,16.5265840124582));
#36381=CARTESIAN_POINT('',(-9.625,37.03,16.6709890228504));
#36382=CARTESIAN_POINT('',(-10.1146191541229,37.03,16.3785524197668));
#36383=CARTESIAN_POINT('',(-9.87089260802485,37.03,16.5265840124582));
#36384=CARTESIAN_POINT('',(-10.1820769523934,37.03,15.7003835976467));
#36385=CARTESIAN_POINT('',(-10.1146191541229,37.03,16.3785524197668));
#36386=CARTESIAN_POINT('',(-10.208136822609,37.03,15.0386712143394));
#36387=CARTESIAN_POINT('',(-10.1820769523934,37.03,15.7003835976467));
#36388=CARTESIAN_POINT('',(-10.192780409838,37.03,14.3959225765489));
#36389=CARTESIAN_POINT('',(-10.208136822609,37.03,15.0386712143394));
#36390=CARTESIAN_POINT('',(-10.1356594341564,37.03,13.7749103120746));
#36391=CARTESIAN_POINT('',(-10.192780409838,37.03,14.3959225765489));
#36392=CARTESIAN_POINT('',(-10.0358241714444,37.03,13.1788877890042));
#36393=CARTESIAN_POINT('',(-10.1356594341564,37.03,13.7749103120746));
#36394=CARTESIAN_POINT('',(-10.0197923273836,37.03,13.1160858846074));
#36395=CARTESIAN_POINT('',(-10.0358241714444,37.03,13.1788877890042));
#36396=CARTESIAN_POINT('',(-7.86882139091926,37.03,10.47057043093));
#36397=CARTESIAN_POINT('',(-3.73232656247359,37.03,5.38302563560253));
#36398=CARTESIAN_POINT('',(-9.23658232924928,37.03,9.23658232924928));
#36399=CARTESIAN_POINT('',(-8.24055326038936,37.03,10.1351955192135));
#36400=CARTESIAN_POINT('',(-10.47057043093,37.03,7.86882139091926));
#36401=CARTESIAN_POINT('',(-9.23658232924928,37.03,9.23658232924928));
#36402=CARTESIAN_POINT('',(-13.1160858846074,37.03,10.0197923273836));
#36403=CARTESIAN_POINT('',(-6.11686363738663,37.03,4.32898314662489));
#36404=CARTESIAN_POINT('',(-13.1788877890042,37.03,10.0358241714444));
#36405=CARTESIAN_POINT('',(-12.6120676561534,37.03,9.89112836854343));
#36406=CARTESIAN_POINT('',(-13.7749103120746,37.03,10.1356594341564));
#36407=CARTESIAN_POINT('',(-13.1788877890042,37.03,10.0358241714444));
#36408=CARTESIAN_POINT('',(-14.3959225765489,37.03,10.192780409838));
#36409=CARTESIAN_POINT('',(-13.7749103120746,37.03,10.1356594341564));
#36410=CARTESIAN_POINT('',(-15.0386712143394,37.03,10.208136822609));
#36411=CARTESIAN_POINT('',(-14.3959225765489,37.03,10.192780409838));
#36412=CARTESIAN_POINT('',(-15.7003835976467,37.03,10.1820769523934));
#36413=CARTESIAN_POINT('',(-15.0386712143394,37.03,10.208136822609));
#36414=CARTESIAN_POINT('',(-16.3785524197668,37.03,10.1146191541229));
#36415=CARTESIAN_POINT('',(-15.7003835976467,37.03,10.1820769523934));
#36416=CARTESIAN_POINT('',(-16.5265840124582,37.03,9.87089260802485));
#36417=CARTESIAN_POINT('',(-16.3785524197668,37.03,10.1146191541229));
#36418=CARTESIAN_POINT('',(-16.6709890228504,37.03,9.625));
#36419=CARTESIAN_POINT('',(-16.5265840124582,37.03,9.87089260802485));
#36420=CARTESIAN_POINT('',(-16.8117357628067,37.03,9.37699528855417));
#36421=CARTESIAN_POINT('',(-16.6709890228504,37.03,9.625));
#36422=CARTESIAN_POINT('',(-16.9487933469585,37.03,9.12693289567172));
#36423=CARTESIAN_POINT('',(-16.8117357628067,37.03,9.37699528855417));
#36424=CARTESIAN_POINT('',(-16.6681291028841,37.03,8.50589256852586));
#36425=CARTESIAN_POINT('',(-16.9487933469585,37.03,9.12693289567172));
#36426=CARTESIAN_POINT('',(-16.3598414208564,37.03,7.91980289947518));
#36427=CARTESIAN_POINT('',(-16.6681291028841,37.03,8.50589256852586));
#36428=CARTESIAN_POINT('',(-16.0251680583905,37.03,7.37084445728621));
#36429=CARTESIAN_POINT('',(-16.3598414208564,37.03,7.91980289947518));
#36430=CARTESIAN_POINT('',(-15.6651937101241,37.03,6.86159254803069));
#36431=CARTESIAN_POINT('',(-16.0251680583905,37.03,7.37084445728621));
#36432=CARTESIAN_POINT('',(-15.2807225748869,37.03,6.39533953317997));
#36433=CARTESIAN_POINT('',(-15.6651937101241,37.03,6.86159254803069));
#36434=CARTESIAN_POINT('',(-15.2354376384623,37.03,6.34896741059668));
#36435=CARTESIAN_POINT('',(-15.2807225748869,37.03,6.39533953317997));
#36436=CARTESIAN_POINT('',(-12.0498844378435,37.03,5.13336928983991));
#36437=CARTESIAN_POINT('',(-5.92380243612285,37.03,2.79567366841787));
#36438=CARTESIAN_POINT('',(-12.617406105901,37.03,3.38082377665168));
#36439=CARTESIAN_POINT('',(-12.2041262243426,37.03,4.65706016176645));
#36440=CARTESIAN_POINT('',(-13.0021906807592,37.03,1.57931400691349));
#36441=CARTESIAN_POINT('',(-12.617406105901,37.03,3.38082377665168));
#36442=CARTESIAN_POINT('',(-16.3687597379803,37.03,2.1193517538549));
#36443=CARTESIAN_POINT('',(-7.46185087477454,37.03,0.690577558838538));
#36444=CARTESIAN_POINT('',(-16.4311637046244,37.03,2.10183478588268));
#36445=CARTESIAN_POINT('',(-15.8679351687486,37.03,2.25993461117486));
#36446=CARTESIAN_POINT('',(-16.997251982187,37.03,1.8902833980495));
#36447=CARTESIAN_POINT('',(-16.4311637046244,37.03,2.10183478588268));
#36448=CARTESIAN_POINT('',(-17.5636248671243,37.03,1.62924548184169));
#36449=CARTESIAN_POINT('',(-16.997251982187,37.03,1.8902833980495));
#36450=CARTESIAN_POINT('',(-18.1279397220842,37.03,1.32117020651705));
#36451=CARTESIAN_POINT('',(-17.5636248671243,37.03,1.62924548184169));
#36452=CARTESIAN_POINT('',(-18.6879695209193,37.03,0.96774550523739));
#36453=CARTESIAN_POINT('',(-18.1279397220842,37.03,1.32117020651705));
#36454=CARTESIAN_POINT('',(-19.2415520497946,37.03,0.570240927191683));
#36455=CARTESIAN_POINT('',(-18.6879695209193,37.03,0.96774550523739));
#36456=CARTESIAN_POINT('',(-19.247887896579,37.03,0.285151750348435));
#36457=CARTESIAN_POINT('',(-19.2415520497946,37.03,0.570240927191683));
#36458=CARTESIAN_POINT('',(-19.25,37.03,2.35744508835865E-15));
#36459=CARTESIAN_POINT('',(-19.247887896579,37.03,0.285151750348435));
#36460=CARTESIAN_POINT('',(-19.247887896579,37.03,-0.285151750348431));
#36461=CARTESIAN_POINT('',(-19.25,37.03,2.35744508835865E-15));
#36462=CARTESIAN_POINT('',(-19.2415520497946,37.03,-0.570240927191679));
#36463=CARTESIAN_POINT('',(-19.247887896579,37.03,-0.285151750348431));
#36464=CARTESIAN_POINT('',(-18.6879695209193,37.03,-0.967745505237385));
#36465=CARTESIAN_POINT('',(-19.2415520497946,37.03,-0.570240927191679));
#36466=CARTESIAN_POINT('',(-18.1279397220842,37.03,-1.32117020651705));
#36467=CARTESIAN_POINT('',(-18.6879695209193,37.03,-0.967745505237385));
#36468=CARTESIAN_POINT('',(-17.5636248671243,37.03,-1.62924548184168));
#36469=CARTESIAN_POINT('',(-18.1279397220842,37.03,-1.32117020651705));
#36470=CARTESIAN_POINT('',(-16.997251982187,37.03,-1.89028339804949));
#36471=CARTESIAN_POINT('',(-17.5636248671243,37.03,-1.62924548184168));
#36472=CARTESIAN_POINT('',(-16.4311637046244,37.03,-2.10183478588267));
#36473=CARTESIAN_POINT('',(-16.997251982187,37.03,-1.89028339804949));
#36474=CARTESIAN_POINT('',(-16.3687597379803,37.03,-2.11935175385489));
#36475=CARTESIAN_POINT('',(-16.4311637046244,37.03,-2.10183478588267));
#36476=CARTESIAN_POINT('',(-13.0021906807592,37.03,-1.57931400691349));
#36477=CARTESIAN_POINT('',(-6.52800023089146,37.03,-0.540776800520311));
#36478=CARTESIAN_POINT('',(-12.617406105901,37.03,-3.38082377665168));
#36479=CARTESIAN_POINT('',(-12.8976134221558,37.03,-2.0689307051291));
#36480=CARTESIAN_POINT('',(-12.0498844378435,37.03,-5.13336928983991));
#36481=CARTESIAN_POINT('',(-12.617406105901,37.03,-3.38082377665168));
#36482=CARTESIAN_POINT('',(-15.2354376384623,37.03,-6.34896741059669));
#36483=CARTESIAN_POINT('',(-6.80744119622516,37.03,-3.13286772814966));
#36484=CARTESIAN_POINT('',(-15.2807225748869,37.03,-6.39533953317997));
#36485=CARTESIAN_POINT('',(-14.8720022673282,37.03,-5.97680680020517));
#36486=CARTESIAN_POINT('',(-15.6651937101241,37.03,-6.86159254803069));
#36487=CARTESIAN_POINT('',(-15.2807225748869,37.03,-6.39533953317997));
#36488=CARTESIAN_POINT('',(-16.0251680583905,37.03,-7.37084445728622));
#36489=CARTESIAN_POINT('',(-15.6651937101241,37.03,-6.86159254803069));
#36490=CARTESIAN_POINT('',(-16.3598414208564,37.03,-7.91980289947518));
#36491=CARTESIAN_POINT('',(-16.0251680583905,37.03,-7.37084445728622));
#36492=CARTESIAN_POINT('',(-16.6681291028841,37.03,-8.50589256852587));
#36493=CARTESIAN_POINT('',(-16.3598414208564,37.03,-7.91980289947518));
#36494=CARTESIAN_POINT('',(-16.9487933469585,37.03,-9.12693289567173));
#36495=CARTESIAN_POINT('',(-16.6681291028841,37.03,-8.50589256852587));
#36496=CARTESIAN_POINT('',(-16.8117357628067,37.03,-9.37699528855417));
#36497=CARTESIAN_POINT('',(-16.9487933469585,37.03,-9.12693289567173));
#36498=CARTESIAN_POINT('',(-16.6709890228504,37.03,-9.625));
#36499=CARTESIAN_POINT('',(-16.8117357628067,37.03,-9.37699528855417));
#36500=CARTESIAN_POINT('',(-16.5265840124582,37.03,-9.87089260802485));
#36501=CARTESIAN_POINT('',(-16.6709890228504,37.03,-9.625));
#36502=CARTESIAN_POINT('',(-16.3785524197668,37.03,-10.1146191541229));
#36503=CARTESIAN_POINT('',(-16.5265840124582,37.03,-9.87089260802485));
#36504=CARTESIAN_POINT('',(-15.7003835976467,37.03,-10.1820769523934));
#36505=CARTESIAN_POINT('',(-16.3785524197668,37.03,-10.1146191541229));
#36506=CARTESIAN_POINT('',(-15.0386712143394,37.03,-10.208136822609));
#36507=CARTESIAN_POINT('',(-15.7003835976467,37.03,-10.1820769523934));
#36508=CARTESIAN_POINT('',(-14.3959225765489,37.03,-10.192780409838));
#36509=CARTESIAN_POINT('',(-15.0386712143394,37.03,-10.208136822609));
#36510=CARTESIAN_POINT('',(-13.7749103120746,37.03,-10.1356594341564));
#36511=CARTESIAN_POINT('',(-14.3959225765489,37.03,-10.192780409838));
#36512=CARTESIAN_POINT('',(-13.1788877890042,37.03,-10.0358241714444));
#36513=CARTESIAN_POINT('',(-13.7749103120746,37.03,-10.1356594341564));
#36514=CARTESIAN_POINT('',(-13.1160858846074,37.03,-10.0197923273836));
#36515=CARTESIAN_POINT('',(-13.1788877890042,37.03,-10.0358241714444));
#36516=CARTESIAN_POINT('',(-10.47057043093,37.03,-7.86882139091926));
#36517=CARTESIAN_POINT('',(-5.38302563560254,37.03,-3.73232656247359));
#36518=CARTESIAN_POINT('',(-10.1351955192135,37.03,-8.24055326038937));
#36519=CARTESIAN_POINT('',(1.04094977927525E-15,37.03,-8.5));
#36520=CARTESIAN_POINT('Origin',(0.,37.03,0.));
#36521=CARTESIAN_POINT('Origin',(-10.0358241714444,37.03,-13.1788877890042));
#36522=CARTESIAN_POINT('',(-9.89112836854344,64.7518675845618,-12.6120676561534));
#36523=CARTESIAN_POINT('',(-9.89112836854344,37.03,-12.6120676561534));
#36524=CARTESIAN_POINT('',(-10.0197923273836,64.97,-13.1160858846074));
#36525=CARTESIAN_POINT('',(-7.91093399030624,61.3947146828798,-4.85500754770592));
#36526=CARTESIAN_POINT('',(-10.0358241714444,64.97,-13.1788877890042));
#36527=CARTESIAN_POINT('',(-9.89112836854344,64.97,-12.6120676561534));
#36528=CARTESIAN_POINT('',(-10.0358241714444,37.03,-13.1788877890042));
#36529=CARTESIAN_POINT('Origin',(-9.89112836854344,37.03,-12.6120676561534));
#36530=CARTESIAN_POINT('',(-9.69653989065522,64.5678155074499,-12.0809901437375));
#36531=CARTESIAN_POINT('',(-9.69653989065522,37.03,-12.0809901437375));
#36532=CARTESIAN_POINT('',(-7.22739122706622,62.2323640708404,-5.34210537381292));
#36533=CARTESIAN_POINT('Origin',(-6.8965715342494,37.28,-2.89929593438234));
#36534=CARTESIAN_POINT('',(-14.8720022673282,37.2481324154382,-5.97680680020517));
#36535=CARTESIAN_POINT('',(-12.7594118264622,38.5161005118285,-3.81349796890809));
#36536=CARTESIAN_POINT('',(-12.2041262243426,37.53,-4.65706016176646));
#36537=CARTESIAN_POINT('',(-12.1492258527638,37.3520314584495,-4.82659624346733));
#36538=CARTESIAN_POINT('',(-13.9714037445473,37.53,-5.33144828123002));
#36539=CARTESIAN_POINT('',(-6.98570187227364,37.53,-2.66572414061501));
#36540=CARTESIAN_POINT('',(-14.4379449459854,37.4321844925501,-5.61417442201851));
#36541=CARTESIAN_POINT('',(-11.2242343577003,38.1059743550986,-3.66665083902897));
#36542=CARTESIAN_POINT('',(-12.0847770735356,38.4299914950389,-3.64822471929515));
#36543=CARTESIAN_POINT('Origin',(-15.2807225748869,37.03,-6.39533953317997));
#36544=CARTESIAN_POINT('',(-14.8720022673282,64.7518675845618,-5.97680680020517));
#36545=CARTESIAN_POINT('',(-14.8720022673282,37.03,-5.97680680020517));
#36546=CARTESIAN_POINT('',(-15.2354376384623,64.97,-6.34896741059669));
#36547=CARTESIAN_POINT('',(-9.27857357711986,61.3947146828801,-0.249092876725649));
#36548=CARTESIAN_POINT('',(-15.2807225748869,64.97,-6.39533953317997));
#36549=CARTESIAN_POINT('',(-14.8720022673282,64.97,-5.97680680020517));
#36550=CARTESIAN_POINT('',(-15.2807225748869,37.03,-6.39533953317997));
#36551=CARTESIAN_POINT('Origin',(-14.8720022673282,37.03,-5.97680680020517));
#36552=CARTESIAN_POINT('',(-14.4379449459854,64.5678155074499,-5.61417442201851));
#36553=CARTESIAN_POINT('',(-14.4379449459854,37.03,-5.61417442201851));
#36554=CARTESIAN_POINT('',(-8.93015709263458,62.2323640708404,-1.01270334988218));
#36555=CARTESIAN_POINT('Origin',(-7.42225411486777,37.28,0.937421834860659));
#36556=CARTESIAN_POINT('',(-15.8679351687486,37.2481324154382,2.25993461117486));
#36557=CARTESIAN_POINT('',(-12.9567237635179,38.5161005118285,3.07711979487634));
#36558=CARTESIAN_POINT('',(-12.8976134221558,37.53,2.0689307051291));
#36559=CARTESIAN_POINT('',(-12.9348363465418,37.3520314584495,1.89465796572867));
#36560=CARTESIAN_POINT('',(-14.765314709922,37.53,2.36853222176556));
#36561=CARTESIAN_POINT('',(-7.38265735496099,37.53,1.18426611088278));
#36562=CARTESIAN_POINT('',(-15.3107143126737,37.4321844925501,2.35695480224783));
#36563=CARTESIAN_POINT('',(-11.5537975113131,38.1059743550986,2.43670440544354));
#36564=CARTESIAN_POINT('',(-12.2898363044011,38.4299914950389,2.88293325114382));
#36565=CARTESIAN_POINT('Origin',(-16.4311637046244,37.03,2.10183478588268));
#36566=CARTESIAN_POINT('',(-15.8679351687486,64.7518675845618,2.25993461117486));
#36567=CARTESIAN_POINT('',(-15.8679351687486,37.03,2.25993461117486));
#36568=CARTESIAN_POINT('',(-16.3687597379803,64.97,2.1193517538549));
#36569=CARTESIAN_POINT('',(-8.16002686703167,61.39471468288,4.42356602941383));
#36570=CARTESIAN_POINT('',(-16.4311637046244,64.97,2.10183478588268));
#36571=CARTESIAN_POINT('',(-15.8679351687486,64.97,2.25993461117486));
#36572=CARTESIAN_POINT('',(-16.4311637046244,37.03,2.10183478588268));
#36573=CARTESIAN_POINT('Origin',(-15.8679351687486,37.03,2.25993461117486));
#36574=CARTESIAN_POINT('',(-15.3107143126737,64.5678155074499,2.35695480224783));
#36575=CARTESIAN_POINT('',(-15.3107143126737,37.03,2.35695480224783));
#36576=CARTESIAN_POINT('',(-8.24009457694845,62.2323640708404,3.58805171882167));
#36577=CARTESIAN_POINT('Origin',(-5.95914969938874,37.28,4.52295818048543));
#36578=CARTESIAN_POINT('',(-12.6120676561534,37.2481324154382,9.89112836854343));
#36579=CARTESIAN_POINT('',(-9.68229203158586,38.5161005118285,9.14322579460982));
#36580=CARTESIAN_POINT('',(-10.1351955192135,37.53,8.24055326038937));
#36581=CARTESIAN_POINT('',(-10.2545678870352,37.3520314584495,8.10824010307447));
#36582=CARTESIAN_POINT('',(-11.6028715227817,37.53,9.43386642869196));
#36583=CARTESIAN_POINT('',(-5.80143576139086,37.53,4.71693321434598));
#36584=CARTESIAN_POINT('',(-12.0809901437375,37.4321844925501,9.69653989065521));
#36585=CARTESIAN_POINT('',(-8.78752995225676,38.1059743550986,7.88714667228409));
#36586=CARTESIAN_POINT('',(-9.20184382239172,38.4299914950389,8.64161158510596));
#36587=CARTESIAN_POINT('Origin',(-13.1788877890042,37.03,10.0358241714444));
#36588=CARTESIAN_POINT('',(-12.6120676561534,64.7518675845618,9.89112836854343));
#36589=CARTESIAN_POINT('',(-12.6120676561534,37.03,9.89112836854343));
#36590=CARTESIAN_POINT('',(-13.1160858846074,64.97,10.0197923273836));
#36591=CARTESIAN_POINT('',(-4.85500754770607,61.39471468288,7.91093399030606));
#36592=CARTESIAN_POINT('',(-13.1788877890042,64.97,10.0358241714444));
#36593=CARTESIAN_POINT('',(-12.6120676561534,64.97,9.89112836854343));
#36594=CARTESIAN_POINT('',(-13.1788877890042,37.03,10.0358241714444));
#36595=CARTESIAN_POINT('Origin',(-12.6120676561534,37.03,9.89112836854343));
#36596=CARTESIAN_POINT('',(-12.0809901437375,64.5678155074499,9.69653989065521));
#36597=CARTESIAN_POINT('',(-12.0809901437375,37.03,9.69653989065521));
#36598=CARTESIAN_POINT('',(-5.34210537381293,62.2323640708404,7.22739122706621));
#36599=CARTESIAN_POINT('Origin',(-2.89929593438233,37.28,6.8965715342494));
#36600=CARTESIAN_POINT('',(-5.97680680020517,37.2481324154382,14.8720022673282));
#36601=CARTESIAN_POINT('',(-3.81349796890809,38.5161005118285,12.7594118264622));
#36602=CARTESIAN_POINT('',(-4.65706016176645,37.53,12.2041262243426));
#36603=CARTESIAN_POINT('',(-4.82659624346733,37.3520314584495,12.1492258527638));
#36604=CARTESIAN_POINT('',(-5.33144828123002,37.53,13.9714037445473));
#36605=CARTESIAN_POINT('',(-2.66572414061501,37.53,6.98570187227364));
#36606=CARTESIAN_POINT('',(-5.6141744220185,37.4321844925501,14.4379449459854));
#36607=CARTESIAN_POINT('',(-3.66665083902899,38.1059743550985,11.2242343577003));
#36608=CARTESIAN_POINT('',(-3.64822471929515,38.4299914950389,12.0847770735356));
#36609=CARTESIAN_POINT('Origin',(-6.39533953317997,37.03,15.2807225748869));
#36610=CARTESIAN_POINT('',(-5.97680680020517,64.7518675845618,14.8720022673282));
#36611=CARTESIAN_POINT('',(-5.97680680020517,37.03,14.8720022673282));
#36612=CARTESIAN_POINT('',(-6.34896741059669,64.97,15.2354376384623));
#36613=CARTESIAN_POINT('',(-0.24909287672559,61.39471468288,9.27857357711989));
#36614=CARTESIAN_POINT('',(-6.39533953317997,64.97,15.2807225748869));
#36615=CARTESIAN_POINT('',(-5.97680680020517,64.97,14.8720022673282));
#36616=CARTESIAN_POINT('',(-6.39533953317997,37.03,15.2807225748869));
#36617=CARTESIAN_POINT('Origin',(-5.97680680020517,37.03,14.8720022673282));
#36618=CARTESIAN_POINT('',(-5.6141744220185,64.5678155074499,14.4379449459854));
#36619=CARTESIAN_POINT('',(-5.6141744220185,37.03,14.4379449459854));
#36620=CARTESIAN_POINT('',(-1.01270334988219,62.2323640708404,8.93015709263459));
#36621=CARTESIAN_POINT('Origin',(0.937421834860657,37.28,7.42225411486777));
#36622=CARTESIAN_POINT('',(2.25993461117485,37.2481324154382,15.8679351687486));
#36623=CARTESIAN_POINT('',(3.07711979487634,38.5161005118285,12.9567237635179));
#36624=CARTESIAN_POINT('',(2.0689307051291,37.53,12.8976134221558));
#36625=CARTESIAN_POINT('',(1.89465796572866,37.3520314584495,12.9348363465418));
#36626=CARTESIAN_POINT('',(2.36853222176556,37.53,14.765314709922));
#36627=CARTESIAN_POINT('',(1.18426611088278,37.53,7.38265735496099));
#36628=CARTESIAN_POINT('',(2.35695480224784,37.4321844925501,15.3107143126737));
#36629=CARTESIAN_POINT('',(2.4367044054435,38.1059743550985,11.553797511313));
#36630=CARTESIAN_POINT('',(2.88293325114383,38.4299914950389,12.2898363044011));
#36631=CARTESIAN_POINT('Origin',(2.10183478588268,37.03,16.4311637046244));
#36632=CARTESIAN_POINT('',(2.25993461117485,64.7518675845618,15.8679351687486));
#36633=CARTESIAN_POINT('',(2.25993461117485,37.03,15.8679351687486));
#36634=CARTESIAN_POINT('',(2.11935175385489,64.97,16.3687597379803));
#36635=CARTESIAN_POINT('',(4.42356602941384,61.39471468288,8.16002686703167));
#36636=CARTESIAN_POINT('',(2.10183478588268,64.97,16.4311637046244));
#36637=CARTESIAN_POINT('',(2.25993461117485,64.97,15.8679351687486));
#36638=CARTESIAN_POINT('',(2.10183478588268,37.03,16.4311637046244));
#36639=CARTESIAN_POINT('Origin',(2.25993461117485,37.03,15.8679351687486));
#36640=CARTESIAN_POINT('',(2.35695480224784,64.5678155074499,15.3107143126737));
#36641=CARTESIAN_POINT('',(2.35695480224784,37.03,15.3107143126737));
#36642=CARTESIAN_POINT('',(3.58805171882171,62.2323640708404,8.24009457694843));
#36643=CARTESIAN_POINT('Origin',(4.52295818048543,37.28,5.95914969938874));
#36644=CARTESIAN_POINT('',(9.89112836854343,37.2481324154382,12.6120676561534));
#36645=CARTESIAN_POINT('',(9.14322579460982,38.5161005118285,9.68229203158586));
#36646=CARTESIAN_POINT('',(8.24055326038937,37.53,10.1351955192135));
#36647=CARTESIAN_POINT('',(8.10824010307447,37.3520314584495,10.2545678870352));
#36648=CARTESIAN_POINT('',(9.43386642869196,37.53,11.6028715227817));
#36649=CARTESIAN_POINT('',(4.71693321434598,37.53,5.80143576139086));
#36650=CARTESIAN_POINT('',(9.69653989065521,37.4321844925501,12.0809901437375));
#36651=CARTESIAN_POINT('',(7.88714667228404,38.1059743550985,8.78752995225676));
#36652=CARTESIAN_POINT('',(8.641611585106,38.4299914950389,9.20184382239174));
#36653=CARTESIAN_POINT('Origin',(10.0358241714444,37.03,13.1788877890042));
#36654=CARTESIAN_POINT('',(9.89112836854343,64.7518675845618,12.6120676561534));
#36655=CARTESIAN_POINT('',(9.89112836854343,37.03,12.6120676561534));
#36656=CARTESIAN_POINT('',(10.0197923273836,64.97,13.1160858846074));
#36657=CARTESIAN_POINT('',(7.91093399030605,61.3947146828801,4.85500754770609));
#36658=CARTESIAN_POINT('',(10.0358241714444,64.97,13.1788877890042));
#36659=CARTESIAN_POINT('',(9.89112836854343,64.97,12.6120676561534));
#36660=CARTESIAN_POINT('',(10.0358241714444,37.03,13.1788877890042));
#36661=CARTESIAN_POINT('Origin',(9.89112836854343,37.03,12.6120676561534));
#36662=CARTESIAN_POINT('',(9.69653989065521,64.5678155074499,12.0809901437375));
#36663=CARTESIAN_POINT('',(9.69653989065521,37.03,12.0809901437375));
#36664=CARTESIAN_POINT('',(7.22739122706626,62.2323640708404,5.34210537381285));
#36665=CARTESIAN_POINT('Origin',(6.8965715342494,37.28,2.89929593438233));
#36666=CARTESIAN_POINT('',(14.8720022673282,37.2481324154382,5.97680680020517));
#36667=CARTESIAN_POINT('',(12.7594118264622,38.5161005118285,3.81349796890809));
#36668=CARTESIAN_POINT('',(12.2041262243426,37.53,4.65706016176646));
#36669=CARTESIAN_POINT('',(12.1492258527638,37.3520314584495,4.82659624346733));
#36670=CARTESIAN_POINT('',(13.9714037445473,37.53,5.33144828123002));
#36671=CARTESIAN_POINT('',(6.98570187227364,37.53,2.66572414061501));
#36672=CARTESIAN_POINT('',(14.4379449459854,37.4321844925501,5.6141744220185));
#36673=CARTESIAN_POINT('',(11.2242343577003,38.1059743550985,3.66665083902898));
#36674=CARTESIAN_POINT('',(12.0847770735356,38.4299914950389,3.64822471929515));
#36675=CARTESIAN_POINT('Origin',(15.2807225748869,37.03,6.39533953317997));
#36676=CARTESIAN_POINT('',(14.8720022673282,64.7518675845618,5.97680680020517));
#36677=CARTESIAN_POINT('',(14.8720022673282,37.03,5.97680680020517));
#36678=CARTESIAN_POINT('',(15.2354376384623,64.97,6.34896741059669));
#36679=CARTESIAN_POINT('',(9.27857357711988,61.39471468288,0.249092876725602));
#36680=CARTESIAN_POINT('',(15.2807225748869,64.97,6.39533953317997));
#36681=CARTESIAN_POINT('',(14.8720022673282,64.97,5.97680680020517));
#36682=CARTESIAN_POINT('',(15.2807225748869,37.03,6.39533953317997));
#36683=CARTESIAN_POINT('Origin',(14.8720022673282,37.03,5.97680680020517));
#36684=CARTESIAN_POINT('',(14.4379449459854,64.5678155074499,5.6141744220185));
#36685=CARTESIAN_POINT('',(14.4379449459854,37.03,5.6141744220185));
#36686=CARTESIAN_POINT('',(8.93015709263458,62.2323640708404,1.01270334988217));
#36687=CARTESIAN_POINT('Origin',(7.42225411486777,37.28,-0.937421834860657));
#36688=CARTESIAN_POINT('',(15.8679351687486,37.2481324154382,-2.25993461117485));
#36689=CARTESIAN_POINT('',(12.9567237635179,38.5161005118285,-3.07711979487634));
#36690=CARTESIAN_POINT('',(12.8976134221558,37.53,-2.0689307051291));
#36691=CARTESIAN_POINT('',(12.9348363465418,37.3520314584495,-1.89465796572866));
#36692=CARTESIAN_POINT('',(14.765314709922,37.53,-2.36853222176556));
#36693=CARTESIAN_POINT('',(7.38265735496099,37.53,-1.18426611088278));
#36694=CARTESIAN_POINT('',(15.3107143126737,37.4321844925501,-2.35695480224783));
#36695=CARTESIAN_POINT('',(11.553797511313,38.1059743550985,-2.43670440544351));
#36696=CARTESIAN_POINT('',(12.2898363044011,38.4299914950389,-2.88293325114382));
#36697=CARTESIAN_POINT('Origin',(16.4311637046244,37.03,-2.10183478588267));
#36698=CARTESIAN_POINT('',(15.8679351687486,64.7518675845618,-2.25993461117485));
#36699=CARTESIAN_POINT('',(15.8679351687486,37.03,-2.25993461117485));
#36700=CARTESIAN_POINT('',(16.3687597379803,64.97,-2.11935175385489));
#36701=CARTESIAN_POINT('',(8.16002686703167,61.39471468288,-4.42356602941385));
#36702=CARTESIAN_POINT('',(16.4311637046244,64.97,-2.10183478588267));
#36703=CARTESIAN_POINT('',(15.8679351687486,64.97,-2.25993461117485));
#36704=CARTESIAN_POINT('',(16.4311637046244,37.03,-2.10183478588267));
#36705=CARTESIAN_POINT('Origin',(15.8679351687486,37.03,-2.25993461117485));
#36706=CARTESIAN_POINT('',(15.3107143126737,64.5678155074499,-2.35695480224783));
#36707=CARTESIAN_POINT('',(15.3107143126737,37.03,-2.35695480224783));
#36708=CARTESIAN_POINT('',(8.24009457694844,62.2323640708404,-3.58805171882169));
#36709=CARTESIAN_POINT('Origin',(5.95914969938874,37.28,-4.52295818048544));
#36710=CARTESIAN_POINT('',(12.6120676561534,37.2481324154382,-9.89112836854343));
#36711=CARTESIAN_POINT('',(9.68229203158587,38.5161005118285,-9.14322579460984));
#36712=CARTESIAN_POINT('',(10.1351955192135,37.53,-8.24055326038936));
#36713=CARTESIAN_POINT('',(10.2545678870352,37.3520314584495,-8.10824010307447));
#36714=CARTESIAN_POINT('',(11.6028715227817,37.53,-9.43386642869196));
#36715=CARTESIAN_POINT('',(5.80143576139085,37.53,-4.71693321434598));
#36716=CARTESIAN_POINT('',(12.0809901437375,37.4321844925501,-9.69653989065521));
#36717=CARTESIAN_POINT('',(8.78752995225676,38.1059743550985,-7.88714667228404));
#36718=CARTESIAN_POINT('',(9.20184382239173,38.4299914950389,-8.64161158510599));
#36719=CARTESIAN_POINT('Origin',(13.1788877890042,37.03,-10.0358241714444));
#36720=CARTESIAN_POINT('',(12.6120676561534,64.7518675845618,-9.89112836854343));
#36721=CARTESIAN_POINT('',(12.6120676561534,37.03,-9.89112836854343));
#36722=CARTESIAN_POINT('',(13.1160858846074,64.97,-10.0197923273836));
#36723=CARTESIAN_POINT('',(4.85500754770605,61.39471468288,-7.91093399030609));
#36724=CARTESIAN_POINT('',(13.1788877890042,64.97,-10.0358241714444));
#36725=CARTESIAN_POINT('',(12.6120676561534,64.97,-9.89112836854343));
#36726=CARTESIAN_POINT('',(13.1788877890042,37.03,-10.0358241714444));
#36727=CARTESIAN_POINT('Origin',(12.6120676561534,37.03,-9.89112836854343));
#36728=CARTESIAN_POINT('',(12.0809901437375,64.5678155074499,-9.69653989065521));
#36729=CARTESIAN_POINT('',(12.0809901437375,37.03,-9.69653989065521));
#36730=CARTESIAN_POINT('',(5.34210537381288,62.2323640708404,-7.22739122706624));
#36731=CARTESIAN_POINT('Origin',(2.89929593438233,37.28,-6.8965715342494));
#36732=CARTESIAN_POINT('',(5.97680680020517,37.2481324154382,-14.8720022673282));
#36733=CARTESIAN_POINT('',(3.81349796890809,38.5161005118285,-12.7594118264622));
#36734=CARTESIAN_POINT('',(4.65706016176646,37.53,-12.2041262243426));
#36735=CARTESIAN_POINT('',(4.82659624346733,37.3520314584495,-12.1492258527638));
#36736=CARTESIAN_POINT('',(5.33144828123002,37.53,-13.9714037445473));
#36737=CARTESIAN_POINT('',(2.66572414061501,37.53,-6.98570187227364));
#36738=CARTESIAN_POINT('',(5.61417442201851,37.4321844925501,-14.4379449459854));
#36739=CARTESIAN_POINT('',(3.66665083902899,38.1059743550985,-11.2242343577003));
#36740=CARTESIAN_POINT('',(3.64822471929515,38.4299914950389,-12.0847770735356));
#36741=CARTESIAN_POINT('Origin',(6.39533953317997,37.03,-15.2807225748869));
#36742=CARTESIAN_POINT('',(5.97680680020517,64.7518675845618,-14.8720022673282));
#36743=CARTESIAN_POINT('',(5.97680680020517,37.03,-14.8720022673282));
#36744=CARTESIAN_POINT('',(6.34896741059669,64.97,-15.2354376384623));
#36745=CARTESIAN_POINT('',(0.249092876725617,61.39471468288,-9.27857357711988));
#36746=CARTESIAN_POINT('',(6.39533953317997,64.97,-15.2807225748869));
#36747=CARTESIAN_POINT('',(5.97680680020517,64.97,-14.8720022673282));
#36748=CARTESIAN_POINT('',(6.39533953317997,37.03,-15.2807225748869));
#36749=CARTESIAN_POINT('Origin',(5.97680680020517,37.03,-14.8720022673282));
#36750=CARTESIAN_POINT('',(5.61417442201851,64.5678155074499,-14.4379449459854));
#36751=CARTESIAN_POINT('',(5.61417442201851,37.03,-14.4379449459854));
#36752=CARTESIAN_POINT('',(1.01270334988216,62.2323640708403,-8.93015709263459));
#36753=CARTESIAN_POINT('Origin',(-0.937421834860655,37.28,-7.42225411486777));
#36754=CARTESIAN_POINT('',(-2.25993461117485,37.2481324154382,-15.8679351687486));
#36755=CARTESIAN_POINT('',(-3.07711979487634,38.5161005118285,-12.9567237635179));
#36756=CARTESIAN_POINT('',(-2.0689307051291,37.53,-12.8976134221558));
#36757=CARTESIAN_POINT('',(-1.89465796572866,37.3520314584495,-12.9348363465418));
#36758=CARTESIAN_POINT('',(-2.36853222176555,37.53,-14.765314709922));
#36759=CARTESIAN_POINT('',(-1.18426611088278,37.53,-7.38265735496099));
#36760=CARTESIAN_POINT('',(-2.35695480224783,37.4321844925501,-15.3107143126737));
#36761=CARTESIAN_POINT('',(-2.4367044054435,38.1059743550985,-11.553797511313));
#36762=CARTESIAN_POINT('',(-2.88293325114383,38.4299914950389,-12.2898363044011));
#36763=CARTESIAN_POINT('Origin',(-2.10183478588267,37.03,-16.4311637046244));
#36764=CARTESIAN_POINT('',(-2.25993461117485,64.7518675845618,-15.8679351687486));
#36765=CARTESIAN_POINT('',(-2.25993461117485,37.03,-15.8679351687486));
#36766=CARTESIAN_POINT('',(-2.11935175385489,64.97,-16.3687597379803));
#36767=CARTESIAN_POINT('',(-4.42356602941384,61.39471468288,-8.16002686703167));
#36768=CARTESIAN_POINT('',(-2.10183478588267,64.97,-16.4311637046244));
#36769=CARTESIAN_POINT('',(-2.25993461117485,64.97,-15.8679351687486));
#36770=CARTESIAN_POINT('',(-2.10183478588267,37.03,-16.4311637046244));
#36771=CARTESIAN_POINT('Origin',(-2.25993461117485,37.03,-15.8679351687486));
#36772=CARTESIAN_POINT('',(-2.35695480224783,64.5678155074499,-15.3107143126737));
#36773=CARTESIAN_POINT('',(-2.35695480224783,37.03,-15.3107143126737));
#36774=CARTESIAN_POINT('',(-3.58805171882171,62.2323640708404,-8.24009457694843));
#36775=CARTESIAN_POINT('Origin',(-2.56210187465055,37.28,-6.01293277414708));
#36776=CARTESIAN_POINT('',(-5.61417442201851,37.4321844925501,-14.4379449459854));
#36777=CARTESIAN_POINT('',(-5.33144828123003,37.53,-13.9714037445473));
#36778=CARTESIAN_POINT('',(-3.29608808746436,38.2341789260845,-10.6127493678757));
#36779=CARTESIAN_POINT('',(-4.65706016176646,37.53,-12.2041262243426));
#36780=CARTESIAN_POINT('',(-2.32853008088323,37.53,-6.10206311217132));
#36781=CARTESIAN_POINT('',(-4.49554999076345,37.6995434345929,-12.2564275888243));
#36782=CARTESIAN_POINT('',(-5.97680680020517,37.2481324154382,-14.8720022673282));
#36783=CARTESIAN_POINT('',(-3.37431437066651,38.7735167359811,-12.3305248094967));
#36784=CARTESIAN_POINT('',(-3.22502994327358,38.6447816854218,-11.5782288391921));
#36785=CARTESIAN_POINT('Origin',(-4.65706016176646,37.03,-12.2041262243426));
#36786=CARTESIAN_POINT('',(-5.33144828123003,64.47,-13.9714037445473));
#36787=CARTESIAN_POINT('',(-5.33144828123003,37.03,-13.9714037445473));
#36788=CARTESIAN_POINT('',(-4.65706016176646,64.47,-12.2041262243426));
#36789=CARTESIAN_POINT('',(-2.32853008088323,64.47,-6.10206311217132));
#36790=CARTESIAN_POINT('',(-4.65706016176646,37.03,-12.2041262243426));
#36791=CARTESIAN_POINT('Origin',(-5.33144828123003,37.03,-13.9714037445473));
#36792=CARTESIAN_POINT('',(-5.61417442201851,64.5678155074499,-14.4379449459854));
#36793=CARTESIAN_POINT('',(-5.61417442201851,37.03,-14.4379449459854));
#36794=CARTESIAN_POINT('',(-2.03831674197423,63.3306666093445,-8.53723504499476));
#36795=CARTESIAN_POINT('Origin',(-5.22531169760465,37.28,-3.92630159633413));
#36796=CARTESIAN_POINT('',(-12.0809901437375,37.4321844925501,-9.69653989065521));
#36797=CARTESIAN_POINT('',(-11.6028715227817,37.53,-9.43386642869196));
#36798=CARTESIAN_POINT('',(-8.16087070079327,38.2341789260846,-7.54286651284552));
#36799=CARTESIAN_POINT('',(-10.1351955192135,37.53,-8.24055326038937));
#36800=CARTESIAN_POINT('',(-5.06759775960677,37.53,-4.12027663019468));
#36801=CARTESIAN_POINT('',(-10.0214742903962,37.6995434345929,-8.36660265618453));
#36802=CARTESIAN_POINT('',(-12.6120676561534,37.2481324154382,-9.89112836854343));
#36803=CARTESIAN_POINT('',(-9.08750437010039,38.773516735981,-8.99139054168508));
#36804=CARTESIAN_POINT('',(-8.58207227843645,38.6447816854217,-8.41452533393317));
#36805=CARTESIAN_POINT('Origin',(-10.1351955192135,37.03,-8.24055326038937));
#36806=CARTESIAN_POINT('',(-11.6028715227817,64.47,-9.43386642869196));
#36807=CARTESIAN_POINT('',(-11.6028715227817,37.03,-9.43386642869196));
#36808=CARTESIAN_POINT('',(-10.1351955192135,64.47,-8.24055326038937));
#36809=CARTESIAN_POINT('',(-5.06759775960677,64.47,-4.12027663019468));
#36810=CARTESIAN_POINT('',(-10.1351955192135,37.03,-8.24055326038937));
#36811=CARTESIAN_POINT('Origin',(-11.6028715227817,37.03,-9.43386642869196));
#36812=CARTESIAN_POINT('',(-12.0809901437375,64.5678155074499,-9.69653989065521));
#36813=CARTESIAN_POINT('',(-12.0809901437375,37.03,-9.69653989065521));
#36814=CARTESIAN_POINT('',(-6.03385160200604,63.3306666093444,-6.37430405605714));
#36815=CARTESIAN_POINT('Origin',(-6.48840347098469,37.28,-0.787621076542431));
#36816=CARTESIAN_POINT('',(-15.3107143126737,37.4321844925501,-2.35695480224783));
#36817=CARTESIAN_POINT('',(-14.765314709922,37.53,-2.36853222176556));
#36818=CARTESIAN_POINT('',(-10.8389546003099,38.2341789260846,-2.45187866708253));
#36819=CARTESIAN_POINT('',(-12.8976134221558,37.53,-2.0689307051291));
#36820=CARTESIAN_POINT('',(-6.44880671107791,37.53,-1.03446535256455));
#36821=CARTESIAN_POINT('',(-12.862152646948,37.6995434345929,-2.23495329842808));
#36822=CARTESIAN_POINT('',(-15.8679351687486,37.2481324154382,-2.25993461117485));
#36823=CARTESIAN_POINT('',(-12.3657049123516,38.773516735981,-3.24302043939622));
#36824=CARTESIAN_POINT('',(-11.6395552772067,38.6447816854217,-2.99615656075563));
#36825=CARTESIAN_POINT('Origin',(-12.8976134221558,37.03,-2.0689307051291));
#36826=CARTESIAN_POINT('',(-14.765314709922,64.47,-2.36853222176556));
#36827=CARTESIAN_POINT('',(-14.765314709922,37.03,-2.36853222176556));
#36828=CARTESIAN_POINT('',(-12.8976134221558,64.47,-2.0689307051291));
#36829=CARTESIAN_POINT('',(-6.44880671107791,64.47,-1.03446535256455));
#36830=CARTESIAN_POINT('',(-12.8976134221558,37.03,-2.0689307051291));
#36831=CARTESIAN_POINT('Origin',(-14.765314709922,37.03,-2.36853222176556));
#36832=CARTESIAN_POINT('',(-15.3107143126737,64.5678155074499,-2.35695480224783));
#36833=CARTESIAN_POINT('',(-15.3107143126737,37.03,-2.35695480224783));
#36834=CARTESIAN_POINT('',(-8.41262079803121,63.3306666093444,-2.50338344298866));
#36835=CARTESIAN_POINT('Origin',(-6.01293277414708,37.28,2.56210187465055));
#36836=CARTESIAN_POINT('',(-14.4379449459854,37.4321844925501,5.61417442201851));
#36837=CARTESIAN_POINT('',(-13.9714037445473,37.53,5.33144828123002));
#36838=CARTESIAN_POINT('',(-10.6127493678758,38.2341789260846,3.29608808746433));
#36839=CARTESIAN_POINT('',(-12.2041262243426,37.53,4.65706016176645));
#36840=CARTESIAN_POINT('',(-6.10206311217132,37.53,2.32853008088323));
#36841=CARTESIAN_POINT('',(-12.2564275888243,37.6995434345929,4.49554999076345));
#36842=CARTESIAN_POINT('',(-14.8720022673282,37.2481324154382,5.97680680020517));
#36843=CARTESIAN_POINT('',(-12.3305248094966,38.773516735981,3.3743143706665));
#36844=CARTESIAN_POINT('',(-11.5782288391921,38.6447816854218,3.22502994327358));
#36845=CARTESIAN_POINT('Origin',(-12.2041262243426,37.03,4.65706016176645));
#36846=CARTESIAN_POINT('',(-13.9714037445473,64.47,5.33144828123002));
#36847=CARTESIAN_POINT('',(-13.9714037445473,37.03,5.33144828123002));
#36848=CARTESIAN_POINT('',(-12.2041262243426,64.47,4.65706016176645));
#36849=CARTESIAN_POINT('',(-6.10206311217132,64.47,2.32853008088323));
#36850=CARTESIAN_POINT('',(-12.2041262243426,37.03,4.65706016176645));
#36851=CARTESIAN_POINT('Origin',(-13.9714037445473,37.03,5.33144828123002));
#36852=CARTESIAN_POINT('',(-14.4379449459854,64.5678155074499,5.61417442201851));
#36853=CARTESIAN_POINT('',(-14.4379449459854,37.03,5.61417442201851));
#36854=CARTESIAN_POINT('',(-8.53723504499469,63.3306666093444,2.0383167419741));
#36855=CARTESIAN_POINT('Origin',(-3.92630159633414,37.28,5.22531169760465));
#36856=CARTESIAN_POINT('',(-9.6965398906552,37.4321844925501,12.0809901437375));
#36857=CARTESIAN_POINT('',(-9.43386642869196,37.53,11.6028715227817));
#36858=CARTESIAN_POINT('',(-7.54286651284552,38.2341789260846,8.16087070079328));
#36859=CARTESIAN_POINT('',(-8.24055326038936,37.53,10.1351955192135));
#36860=CARTESIAN_POINT('',(-4.12027663019469,37.53,5.06759775960677));
#36861=CARTESIAN_POINT('',(-8.36660265618453,37.6995434345929,10.0214742903962));
#36862=CARTESIAN_POINT('',(-9.89112836854343,37.2481324154382,12.6120676561534));
#36863=CARTESIAN_POINT('',(-8.9913905416851,38.773516735981,9.08750437010041));
#36864=CARTESIAN_POINT('',(-8.41452533393316,38.6447816854217,8.58207227843645));
#36865=CARTESIAN_POINT('Origin',(-8.24055326038936,37.03,10.1351955192135));
#36866=CARTESIAN_POINT('',(-9.43386642869196,64.47,11.6028715227817));
#36867=CARTESIAN_POINT('',(-9.43386642869196,37.03,11.6028715227817));
#36868=CARTESIAN_POINT('',(-8.24055326038936,64.47,10.1351955192135));
#36869=CARTESIAN_POINT('',(-4.12027663019469,64.47,5.06759775960677));
#36870=CARTESIAN_POINT('',(-8.24055326038936,37.03,10.1351955192135));
#36871=CARTESIAN_POINT('Origin',(-9.43386642869196,37.03,11.6028715227817));
#36872=CARTESIAN_POINT('',(-9.6965398906552,64.5678155074499,12.0809901437375));
#36873=CARTESIAN_POINT('',(-9.6965398906552,37.03,12.0809901437375));
#36874=CARTESIAN_POINT('',(-6.37430405605714,63.3306666093444,6.03385160200603));
#36875=CARTESIAN_POINT('Origin',(-0.787621076542428,37.28,6.48840347098469));
#36876=CARTESIAN_POINT('',(-2.35695480224783,37.4321844925501,15.3107143126737));
#36877=CARTESIAN_POINT('',(-2.36853222176555,37.53,14.765314709922));
#36878=CARTESIAN_POINT('',(-2.45187866708248,38.2341789260845,10.8389546003098));
#36879=CARTESIAN_POINT('',(-2.0689307051291,37.53,12.8976134221558));
#36880=CARTESIAN_POINT('',(-1.03446535256455,37.53,6.44880671107791));
#36881=CARTESIAN_POINT('',(-2.23495329842808,37.6995434345929,12.862152646948));
#36882=CARTESIAN_POINT('',(-2.25993461117485,37.2481324154382,15.8679351687486));
#36883=CARTESIAN_POINT('',(-3.24302043939622,38.773516735981,12.3657049123516));
#36884=CARTESIAN_POINT('',(-2.99615656075565,38.6447816854218,11.6395552772068));
#36885=CARTESIAN_POINT('Origin',(-2.0689307051291,37.03,12.8976134221558));
#36886=CARTESIAN_POINT('',(-2.36853222176555,64.47,14.765314709922));
#36887=CARTESIAN_POINT('',(-2.36853222176555,37.03,14.765314709922));
#36888=CARTESIAN_POINT('',(-2.0689307051291,64.47,12.8976134221558));
#36889=CARTESIAN_POINT('',(-1.03446535256455,64.47,6.44880671107791));
#36890=CARTESIAN_POINT('',(-2.0689307051291,37.03,12.8976134221558));
#36891=CARTESIAN_POINT('Origin',(-2.36853222176555,37.03,14.765314709922));
#36892=CARTESIAN_POINT('',(-2.35695480224783,64.5678155074499,15.3107143126737));
#36893=CARTESIAN_POINT('',(-2.35695480224783,37.03,15.3107143126737));
#36894=CARTESIAN_POINT('',(-2.50338344298858,63.3306666093445,8.41262079803133));
#36895=CARTESIAN_POINT('Origin',(2.56210187465055,37.28,6.01293277414708));
#36896=CARTESIAN_POINT('',(5.61417442201851,37.4321844925501,14.4379449459854));
#36897=CARTESIAN_POINT('',(5.33144828123002,37.53,13.9714037445473));
#36898=CARTESIAN_POINT('',(3.29608808746436,38.2341789260845,10.6127493678757));
#36899=CARTESIAN_POINT('',(4.65706016176646,37.53,12.2041262243426));
#36900=CARTESIAN_POINT('',(2.32853008088323,37.53,6.10206311217132));
#36901=CARTESIAN_POINT('',(4.49554999076345,37.6995434345929,12.2564275888243));
#36902=CARTESIAN_POINT('',(5.97680680020517,37.2481324154382,14.8720022673282));
#36903=CARTESIAN_POINT('',(3.37431437066651,38.773516735981,12.3305248094966));
#36904=CARTESIAN_POINT('',(3.22502994327357,38.6447816854218,11.5782288391921));
#36905=CARTESIAN_POINT('Origin',(4.65706016176646,37.03,12.2041262243426));
#36906=CARTESIAN_POINT('',(5.33144828123002,64.47,13.9714037445473));
#36907=CARTESIAN_POINT('',(5.33144828123002,37.03,13.9714037445473));
#36908=CARTESIAN_POINT('',(4.65706016176646,64.47,12.2041262243426));
#36909=CARTESIAN_POINT('',(2.32853008088323,64.47,6.10206311217132));
#36910=CARTESIAN_POINT('',(4.65706016176646,37.03,12.2041262243426));
#36911=CARTESIAN_POINT('Origin',(5.33144828123002,37.03,13.9714037445473));
#36912=CARTESIAN_POINT('',(5.61417442201851,64.5678155074499,14.4379449459854));
#36913=CARTESIAN_POINT('',(5.61417442201851,37.03,14.4379449459854));
#36914=CARTESIAN_POINT('',(2.03831674197423,63.3306666093445,8.53723504499476));
#36915=CARTESIAN_POINT('Origin',(5.22531169760465,37.28,3.92630159633414));
#36916=CARTESIAN_POINT('',(12.0809901437375,37.4321844925501,9.69653989065521));
#36917=CARTESIAN_POINT('',(11.6028715227817,37.53,9.43386642869196));
#36918=CARTESIAN_POINT('',(8.16087070079327,38.2341789260845,7.54286651284547));
#36919=CARTESIAN_POINT('',(10.1351955192135,37.53,8.24055326038936));
#36920=CARTESIAN_POINT('',(5.06759775960677,37.53,4.12027663019469));
#36921=CARTESIAN_POINT('',(10.0214742903962,37.6995434345929,8.36660265618453));
#36922=CARTESIAN_POINT('',(12.6120676561534,37.2481324154382,9.89112836854343));
#36923=CARTESIAN_POINT('',(9.08750437010041,38.773516735981,8.9913905416851));
#36924=CARTESIAN_POINT('',(8.58207227843646,38.6447816854218,8.41452533393319));
#36925=CARTESIAN_POINT('Origin',(10.1351955192135,37.03,8.24055326038936));
#36926=CARTESIAN_POINT('',(11.6028715227817,64.47,9.43386642869196));
#36927=CARTESIAN_POINT('',(11.6028715227817,37.03,9.43386642869196));
#36928=CARTESIAN_POINT('',(10.1351955192135,64.47,8.24055326038936));
#36929=CARTESIAN_POINT('',(5.06759775960677,64.47,4.12027663019469));
#36930=CARTESIAN_POINT('',(10.1351955192135,37.03,8.24055326038936));
#36931=CARTESIAN_POINT('Origin',(11.6028715227817,37.03,9.43386642869196));
#36932=CARTESIAN_POINT('',(12.0809901437375,64.5678155074499,9.69653989065521));
#36933=CARTESIAN_POINT('',(12.0809901437375,37.03,9.69653989065521));
#36934=CARTESIAN_POINT('',(6.03385160200616,63.3306666093445,6.37430405605714));
#36935=CARTESIAN_POINT('Origin',(6.48840347098469,37.28,0.78762107654243));
#36936=CARTESIAN_POINT('',(15.3107143126737,37.4321844925501,2.35695480224783));
#36937=CARTESIAN_POINT('',(14.765314709922,37.53,2.36853222176556));
#36938=CARTESIAN_POINT('',(10.8389546003098,38.2341789260845,2.4518786670825));
#36939=CARTESIAN_POINT('',(12.8976134221558,37.53,2.0689307051291));
#36940=CARTESIAN_POINT('',(6.44880671107791,37.53,1.03446535256455));
#36941=CARTESIAN_POINT('',(12.862152646948,37.6995434345929,2.23495329842808));
#36942=CARTESIAN_POINT('',(15.8679351687486,37.2481324154382,2.25993461117485));
#36943=CARTESIAN_POINT('',(12.3657049123516,38.773516735981,3.24302043939622));
#36944=CARTESIAN_POINT('',(11.6395552772068,38.6447816854218,2.99615656075564));
#36945=CARTESIAN_POINT('Origin',(12.8976134221558,37.03,2.0689307051291));
#36946=CARTESIAN_POINT('',(14.765314709922,64.47,2.36853222176556));
#36947=CARTESIAN_POINT('',(14.765314709922,37.03,2.36853222176556));
#36948=CARTESIAN_POINT('',(12.8976134221558,64.47,2.0689307051291));
#36949=CARTESIAN_POINT('',(6.44880671107791,64.47,1.03446535256455));
#36950=CARTESIAN_POINT('',(12.8976134221558,37.03,2.0689307051291));
#36951=CARTESIAN_POINT('Origin',(14.765314709922,37.03,2.36853222176556));
#36952=CARTESIAN_POINT('',(15.3107143126737,64.5678155074499,2.35695480224783));
#36953=CARTESIAN_POINT('',(15.3107143126737,37.03,2.35695480224783));
#36954=CARTESIAN_POINT('',(8.4126207980313,63.3306666093445,2.5033834429886));
#36955=CARTESIAN_POINT('Origin',(6.01293277414708,37.28,-2.56210187465055));
#36956=CARTESIAN_POINT('',(14.4379449459854,37.4321844925501,-5.6141744220185));
#36957=CARTESIAN_POINT('',(13.9714037445473,37.53,-5.33144828123002));
#36958=CARTESIAN_POINT('',(10.6127493678758,38.2341789260845,-3.29608808746435));
#36959=CARTESIAN_POINT('',(12.2041262243426,37.53,-4.65706016176646));
#36960=CARTESIAN_POINT('',(6.10206311217132,37.53,-2.32853008088323));
#36961=CARTESIAN_POINT('',(12.2564275888243,37.6995434345929,-4.49554999076345));
#36962=CARTESIAN_POINT('',(14.8720022673282,37.2481324154382,-5.97680680020517));
#36963=CARTESIAN_POINT('',(12.3305248094966,38.773516735981,-3.3743143706665));
#36964=CARTESIAN_POINT('',(11.5782288391921,38.6447816854218,-3.22502994327357));
#36965=CARTESIAN_POINT('Origin',(12.2041262243426,37.03,-4.65706016176646));
#36966=CARTESIAN_POINT('',(13.9714037445473,64.47,-5.33144828123002));
#36967=CARTESIAN_POINT('',(13.9714037445473,37.03,-5.33144828123002));
#36968=CARTESIAN_POINT('',(12.2041262243426,64.47,-4.65706016176646));
#36969=CARTESIAN_POINT('',(6.10206311217132,64.47,-2.32853008088323));
#36970=CARTESIAN_POINT('',(12.2041262243426,37.03,-4.65706016176646));
#36971=CARTESIAN_POINT('Origin',(13.9714037445473,37.03,-5.33144828123002));
#36972=CARTESIAN_POINT('',(14.4379449459854,64.5678155074499,-5.6141744220185));
#36973=CARTESIAN_POINT('',(14.4379449459854,37.03,-5.6141744220185));
#36974=CARTESIAN_POINT('',(8.53723504499474,63.3306666093445,-2.03831674197418));
#36975=CARTESIAN_POINT('Origin',(3.92630159633414,37.28,-5.22531169760465));
#36976=CARTESIAN_POINT('',(9.69653989065521,37.4321844925501,-12.0809901437375));
#36977=CARTESIAN_POINT('',(9.43386642869196,37.53,-11.6028715227817));
#36978=CARTESIAN_POINT('',(7.54286651284547,38.2341789260845,-8.16087070079327));
#36979=CARTESIAN_POINT('',(8.24055326038937,37.53,-10.1351955192135));
#36980=CARTESIAN_POINT('',(4.12027663019468,37.53,-5.06759775960677));
#36981=CARTESIAN_POINT('',(8.36660265618453,37.6995434345929,-10.0214742903962));
#36982=CARTESIAN_POINT('',(9.89112836854343,37.2481324154382,-12.6120676561534));
#36983=CARTESIAN_POINT('',(8.99139054168508,38.773516735981,-9.08750437010039));
#36984=CARTESIAN_POINT('',(8.41452533393321,38.6447816854218,-8.58207227843647));
#36985=CARTESIAN_POINT('Origin',(8.24055326038937,37.03,-10.1351955192135));
#36986=CARTESIAN_POINT('',(9.43386642869196,64.47,-11.6028715227817));
#36987=CARTESIAN_POINT('',(9.43386642869196,37.03,-11.6028715227817));
#36988=CARTESIAN_POINT('',(8.24055326038937,64.47,-10.1351955192135));
#36989=CARTESIAN_POINT('',(4.12027663019468,64.47,-5.06759775960677));
#36990=CARTESIAN_POINT('',(8.24055326038937,37.03,-10.1351955192135));
#36991=CARTESIAN_POINT('Origin',(9.43386642869196,37.03,-11.6028715227817));
#36992=CARTESIAN_POINT('',(9.69653989065521,64.5678155074499,-12.0809901437375));
#36993=CARTESIAN_POINT('',(9.69653989065521,37.03,-12.0809901437375));
#36994=CARTESIAN_POINT('',(6.37430405605713,63.3306666093445,-6.03385160200617));
#36995=CARTESIAN_POINT('Origin',(0.78762107654243,37.28,-6.48840347098469));
#36996=CARTESIAN_POINT('',(2.35695480224784,37.4321844925501,-15.3107143126737));
#36997=CARTESIAN_POINT('',(2.36853222176556,37.53,-14.765314709922));
#36998=CARTESIAN_POINT('',(2.45187866708248,38.2341789260845,-10.8389546003098));
#36999=CARTESIAN_POINT('',(2.0689307051291,37.53,-12.8976134221558));
#37000=CARTESIAN_POINT('',(1.03446535256455,37.53,-6.44880671107791));
#37001=CARTESIAN_POINT('',(2.23495329842808,37.6995434345929,-12.862152646948));
#37002=CARTESIAN_POINT('',(2.25993461117485,37.2481324154382,-15.8679351687486));
#37003=CARTESIAN_POINT('',(3.24302043939622,38.773516735981,-12.3657049123516));
#37004=CARTESIAN_POINT('',(2.99615656075565,38.6447816854218,-11.6395552772068));
#37005=CARTESIAN_POINT('Origin',(2.0689307051291,37.03,-12.8976134221558));
#37006=CARTESIAN_POINT('',(2.36853222176556,64.47,-14.765314709922));
#37007=CARTESIAN_POINT('',(2.36853222176556,37.03,-14.765314709922));
#37008=CARTESIAN_POINT('',(2.0689307051291,64.47,-12.8976134221558));
#37009=CARTESIAN_POINT('',(1.03446535256455,64.47,-6.44880671107791));
#37010=CARTESIAN_POINT('',(2.0689307051291,37.03,-12.8976134221558));
#37011=CARTESIAN_POINT('Origin',(2.36853222176556,37.03,-14.765314709922));
#37012=CARTESIAN_POINT('',(2.35695480224784,64.5678155074499,-15.3107143126737));
#37013=CARTESIAN_POINT('',(2.35695480224784,37.03,-15.3107143126737));
#37014=CARTESIAN_POINT('',(2.50338344298858,63.3306666093445,-8.41262079803134));
#37015=CARTESIAN_POINT('Origin',(-0.937421834860655,64.72,-7.42225411486777));
#37016=CARTESIAN_POINT('',(-2.36853222176555,64.47,-14.765314709922));
#37017=CARTESIAN_POINT('',(-2.4882091813496,63.4588711803305,-9.12746370903454));
#37018=CARTESIAN_POINT('',(-2.0689307051291,64.47,-12.8976134221558));
#37019=CARTESIAN_POINT('',(-1.18426611088278,64.47,-7.38265735496099));
#37020=CARTESIAN_POINT('',(-1.57931400691349,64.97,-13.0021906807592));
#37021=CARTESIAN_POINT('',(-8.72557394122276,57.6721893244721,-11.4758206122532));
#37022=CARTESIAN_POINT('',(-0.690577558838534,64.97,-7.46185087477454));
#37023=CARTESIAN_POINT('Origin',(0.,64.97,0.));
#37024=CARTESIAN_POINT('',(-3.38082377665168,64.97,-12.617406105901));
#37025=CARTESIAN_POINT('',(-3.38082377665168,64.97,-12.617406105901));
#37026=CARTESIAN_POINT('',(-5.13336928983992,64.97,-12.0498844378435));
#37027=CARTESIAN_POINT('',(-4.65706016176646,64.97,-12.2041262243426));
#37028=CARTESIAN_POINT('',(-6.34896741059669,64.97,-15.2354376384622));
#37029=CARTESIAN_POINT('',(-2.79567366841787,64.97,-5.92380243612285));
#37030=CARTESIAN_POINT('',(-6.39533953317998,64.97,-15.2807225748869));
#37031=CARTESIAN_POINT('',(-6.39533953317998,64.97,-15.2807225748869));
#37032=CARTESIAN_POINT('',(-6.86159254803069,64.97,-15.6651937101241));
#37033=CARTESIAN_POINT('',(-6.86159254803069,64.97,-15.6651937101241));
#37034=CARTESIAN_POINT('',(-7.37084445728623,64.97,-16.0251680583905));
#37035=CARTESIAN_POINT('',(-7.37084445728623,64.97,-16.0251680583905));
#37036=CARTESIAN_POINT('',(-7.91980289947518,64.97,-16.3598414208564));
#37037=CARTESIAN_POINT('',(-7.91980289947518,64.97,-16.3598414208564));
#37038=CARTESIAN_POINT('',(-8.50589256852587,64.97,-16.6681291028841));
#37039=CARTESIAN_POINT('',(-8.50589256852587,64.97,-16.6681291028841));
#37040=CARTESIAN_POINT('',(-9.12693289567173,64.97,-16.9487933469585));
#37041=CARTESIAN_POINT('',(-9.12693289567173,64.97,-16.9487933469585));
#37042=CARTESIAN_POINT('',(-9.37699528855417,64.97,-16.8117357628067));
#37043=CARTESIAN_POINT('',(-9.37699528855417,64.97,-16.8117357628067));
#37044=CARTESIAN_POINT('',(-9.62500000000001,64.97,-16.6709890228504));
#37045=CARTESIAN_POINT('',(-9.62500000000001,64.97,-16.6709890228504));
#37046=CARTESIAN_POINT('',(-9.87089260802487,64.97,-16.5265840124582));
#37047=CARTESIAN_POINT('',(-9.87089260802487,64.97,-16.5265840124582));
#37048=CARTESIAN_POINT('',(-10.1146191541229,64.97,-16.3785524197668));
#37049=CARTESIAN_POINT('',(-10.1146191541229,64.97,-16.3785524197668));
#37050=CARTESIAN_POINT('',(-10.1820769523934,64.97,-15.7003835976467));
#37051=CARTESIAN_POINT('',(-10.1820769523934,64.97,-15.7003835976467));
#37052=CARTESIAN_POINT('',(-10.208136822609,64.97,-15.0386712143394));
#37053=CARTESIAN_POINT('',(-10.208136822609,64.97,-15.0386712143394));
#37054=CARTESIAN_POINT('',(-10.192780409838,64.97,-14.3959225765489));
#37055=CARTESIAN_POINT('',(-10.192780409838,64.97,-14.3959225765489));
#37056=CARTESIAN_POINT('',(-10.1356594341564,64.97,-13.7749103120746));
#37057=CARTESIAN_POINT('',(-10.1356594341564,64.97,-13.7749103120746));
#37058=CARTESIAN_POINT('',(-10.0358241714444,64.97,-13.1788877890042));
#37059=CARTESIAN_POINT('',(-7.86882139091927,64.97,-10.47057043093));
#37060=CARTESIAN_POINT('',(-4.32898314662489,64.97,-6.11686363738662));
#37061=CARTESIAN_POINT('',(-9.23658232924928,64.97,-9.23658232924928));
#37062=CARTESIAN_POINT('',(-9.23658232924928,64.97,-9.23658232924928));
#37063=CARTESIAN_POINT('',(-10.47057043093,64.97,-7.86882139091926));
#37064=CARTESIAN_POINT('',(-10.1351955192135,64.97,-8.24055326038937));
#37065=CARTESIAN_POINT('',(-13.1160858846074,64.97,-10.0197923273836));
#37066=CARTESIAN_POINT('',(-5.38302563560254,64.97,-3.73232656247359));
#37067=CARTESIAN_POINT('',(-13.1788877890042,64.97,-10.0358241714444));
#37068=CARTESIAN_POINT('',(-13.1788877890042,64.97,-10.0358241714444));
#37069=CARTESIAN_POINT('',(-13.7749103120746,64.97,-10.1356594341564));
#37070=CARTESIAN_POINT('',(-13.7749103120746,64.97,-10.1356594341564));
#37071=CARTESIAN_POINT('',(-14.3959225765489,64.97,-10.192780409838));
#37072=CARTESIAN_POINT('',(-14.3959225765489,64.97,-10.192780409838));
#37073=CARTESIAN_POINT('',(-15.0386712143394,64.97,-10.208136822609));
#37074=CARTESIAN_POINT('',(-15.0386712143394,64.97,-10.208136822609));
#37075=CARTESIAN_POINT('',(-15.7003835976467,64.97,-10.1820769523934));
#37076=CARTESIAN_POINT('',(-15.7003835976467,64.97,-10.1820769523934));
#37077=CARTESIAN_POINT('',(-16.3785524197668,64.97,-10.1146191541229));
#37078=CARTESIAN_POINT('',(-16.3785524197668,64.97,-10.1146191541229));
#37079=CARTESIAN_POINT('',(-16.5265840124582,64.97,-9.87089260802485));
#37080=CARTESIAN_POINT('',(-16.5265840124582,64.97,-9.87089260802485));
#37081=CARTESIAN_POINT('',(-16.6709890228504,64.97,-9.625));
#37082=CARTESIAN_POINT('',(-16.6709890228504,64.97,-9.625));
#37083=CARTESIAN_POINT('',(-16.8117357628067,64.97,-9.37699528855417));
#37084=CARTESIAN_POINT('',(-16.8117357628067,64.97,-9.37699528855417));
#37085=CARTESIAN_POINT('',(-16.9487933469585,64.97,-9.12693289567173));
#37086=CARTESIAN_POINT('',(-16.9487933469585,64.97,-9.12693289567173));
#37087=CARTESIAN_POINT('',(-16.6681291028841,64.97,-8.50589256852587));
#37088=CARTESIAN_POINT('',(-16.6681291028841,64.97,-8.50589256852587));
#37089=CARTESIAN_POINT('',(-16.3598414208564,64.97,-7.91980289947518));
#37090=CARTESIAN_POINT('',(-16.3598414208564,64.97,-7.91980289947518));
#37091=CARTESIAN_POINT('',(-16.0251680583905,64.97,-7.37084445728622));
#37092=CARTESIAN_POINT('',(-16.0251680583905,64.97,-7.37084445728622));
#37093=CARTESIAN_POINT('',(-15.6651937101241,64.97,-6.86159254803069));
#37094=CARTESIAN_POINT('',(-15.6651937101241,64.97,-6.86159254803069));
#37095=CARTESIAN_POINT('',(-15.2807225748869,64.97,-6.39533953317997));
#37096=CARTESIAN_POINT('',(-12.0498844378435,64.97,-5.13336928983991));
#37097=CARTESIAN_POINT('',(-6.80744119622516,64.97,-3.13286772814966));
#37098=CARTESIAN_POINT('',(-12.617406105901,64.97,-3.38082377665168));
#37099=CARTESIAN_POINT('',(-12.617406105901,64.97,-3.38082377665168));
#37100=CARTESIAN_POINT('',(-13.0021906807592,64.97,-1.57931400691349));
#37101=CARTESIAN_POINT('',(-12.8976134221558,64.97,-2.0689307051291));
#37102=CARTESIAN_POINT('',(-16.3687597379803,64.97,-2.11935175385489));
#37103=CARTESIAN_POINT('',(-6.52800023089146,64.97,-0.540776800520311));
#37104=CARTESIAN_POINT('',(-16.4311637046244,64.97,-2.10183478588267));
#37105=CARTESIAN_POINT('',(-16.4311637046244,64.97,-2.10183478588267));
#37106=CARTESIAN_POINT('',(-16.997251982187,64.97,-1.89028339804949));
#37107=CARTESIAN_POINT('',(-16.997251982187,64.97,-1.89028339804949));
#37108=CARTESIAN_POINT('',(-17.5636248671243,64.97,-1.62924548184168));
#37109=CARTESIAN_POINT('',(-17.5636248671243,64.97,-1.62924548184168));
#37110=CARTESIAN_POINT('',(-18.1279397220842,64.97,-1.32117020651705));
#37111=CARTESIAN_POINT('',(-18.1279397220842,64.97,-1.32117020651705));
#37112=CARTESIAN_POINT('',(-18.6879695209193,64.97,-0.967745505237385));
#37113=CARTESIAN_POINT('',(-18.6879695209193,64.97,-0.967745505237385));
#37114=CARTESIAN_POINT('',(-19.2415520497946,64.97,-0.570240927191679));
#37115=CARTESIAN_POINT('',(-19.2415520497946,64.97,-0.570240927191679));
#37116=CARTESIAN_POINT('',(-19.247887896579,64.97,-0.285151750348431));
#37117=CARTESIAN_POINT('',(-19.247887896579,64.97,-0.285151750348431));
#37118=CARTESIAN_POINT('',(-19.25,64.97,2.22044604925031E-15));
#37119=CARTESIAN_POINT('',(-19.25,64.97,2.35744508835865E-15));
#37120=CARTESIAN_POINT('',(-19.247887896579,64.97,0.285151750348436));
#37121=CARTESIAN_POINT('',(-19.247887896579,64.97,0.285151750348435));
#37122=CARTESIAN_POINT('',(-19.2415520497946,64.97,0.570240927191683));
#37123=CARTESIAN_POINT('',(-19.2415520497946,64.97,0.570240927191683));
#37124=CARTESIAN_POINT('',(-18.6879695209193,64.97,0.96774550523739));
#37125=CARTESIAN_POINT('',(-18.6879695209193,64.97,0.96774550523739));
#37126=CARTESIAN_POINT('',(-18.1279397220842,64.97,1.32117020651705));
#37127=CARTESIAN_POINT('',(-18.1279397220842,64.97,1.32117020651705));
#37128=CARTESIAN_POINT('',(-17.5636248671243,64.97,1.62924548184169));
#37129=CARTESIAN_POINT('',(-17.5636248671243,64.97,1.62924548184169));
#37130=CARTESIAN_POINT('',(-16.997251982187,64.97,1.89028339804949));
#37131=CARTESIAN_POINT('',(-16.997251982187,64.97,1.8902833980495));
#37132=CARTESIAN_POINT('',(-16.4311637046244,64.97,2.10183478588268));
#37133=CARTESIAN_POINT('',(-13.0021906807592,64.97,1.57931400691349));
#37134=CARTESIAN_POINT('',(-7.46185087477454,64.97,0.690577558838538));
#37135=CARTESIAN_POINT('',(-12.617406105901,64.97,3.38082377665168));
#37136=CARTESIAN_POINT('',(-12.617406105901,64.97,3.38082377665168));
#37137=CARTESIAN_POINT('',(-12.0498844378435,64.97,5.13336928983991));
#37138=CARTESIAN_POINT('',(-12.2041262243426,64.97,4.65706016176645));
#37139=CARTESIAN_POINT('',(-15.2354376384623,64.97,6.34896741059668));
#37140=CARTESIAN_POINT('',(-5.92380243612285,64.97,2.79567366841787));
#37141=CARTESIAN_POINT('',(-15.2807225748869,64.97,6.39533953317997));
#37142=CARTESIAN_POINT('',(-15.2807225748869,64.97,6.39533953317997));
#37143=CARTESIAN_POINT('',(-15.6651937101241,64.97,6.86159254803069));
#37144=CARTESIAN_POINT('',(-15.6651937101241,64.97,6.86159254803069));
#37145=CARTESIAN_POINT('',(-16.0251680583905,64.97,7.37084445728621));
#37146=CARTESIAN_POINT('',(-16.0251680583905,64.97,7.37084445728621));
#37147=CARTESIAN_POINT('',(-16.3598414208564,64.97,7.91980289947518));
#37148=CARTESIAN_POINT('',(-16.3598414208564,64.97,7.91980289947518));
#37149=CARTESIAN_POINT('',(-16.6681291028841,64.97,8.50589256852586));
#37150=CARTESIAN_POINT('',(-16.6681291028841,64.97,8.50589256852586));
#37151=CARTESIAN_POINT('',(-16.9487933469585,64.97,9.12693289567173));
#37152=CARTESIAN_POINT('',(-16.9487933469585,64.97,9.12693289567172));
#37153=CARTESIAN_POINT('',(-16.8117357628067,64.97,9.37699528855417));
#37154=CARTESIAN_POINT('',(-16.8117357628067,64.97,9.37699528855417));
#37155=CARTESIAN_POINT('',(-16.6709890228504,64.97,9.625));
#37156=CARTESIAN_POINT('',(-16.6709890228504,64.97,9.625));
#37157=CARTESIAN_POINT('',(-16.5265840124582,64.97,9.87089260802485));
#37158=CARTESIAN_POINT('',(-16.5265840124582,64.97,9.87089260802485));
#37159=CARTESIAN_POINT('',(-16.3785524197668,64.97,10.1146191541229));
#37160=CARTESIAN_POINT('',(-16.3785524197668,64.97,10.1146191541229));
#37161=CARTESIAN_POINT('',(-15.7003835976467,64.97,10.1820769523934));
#37162=CARTESIAN_POINT('',(-15.7003835976467,64.97,10.1820769523934));
#37163=CARTESIAN_POINT('',(-15.0386712143394,64.97,10.208136822609));
#37164=CARTESIAN_POINT('',(-15.0386712143394,64.97,10.208136822609));
#37165=CARTESIAN_POINT('',(-14.3959225765489,64.97,10.192780409838));
#37166=CARTESIAN_POINT('',(-14.3959225765489,64.97,10.192780409838));
#37167=CARTESIAN_POINT('',(-13.7749103120746,64.97,10.1356594341564));
#37168=CARTESIAN_POINT('',(-13.7749103120746,64.97,10.1356594341564));
#37169=CARTESIAN_POINT('',(-13.1788877890042,64.97,10.0358241714444));
#37170=CARTESIAN_POINT('',(-10.47057043093,64.97,7.86882139091926));
#37171=CARTESIAN_POINT('',(-6.11686363738663,64.97,4.32898314662489));
#37172=CARTESIAN_POINT('',(-9.23658232924928,64.97,9.23658232924927));
#37173=CARTESIAN_POINT('',(-9.23658232924928,64.97,9.23658232924928));
#37174=CARTESIAN_POINT('',(-7.86882139091926,64.97,10.47057043093));
#37175=CARTESIAN_POINT('',(-8.24055326038936,64.97,10.1351955192135));
#37176=CARTESIAN_POINT('',(-10.0197923273836,64.97,13.1160858846074));
#37177=CARTESIAN_POINT('',(-3.73232656247359,64.97,5.38302563560253));
#37178=CARTESIAN_POINT('',(-10.0358241714444,64.97,13.1788877890042));
#37179=CARTESIAN_POINT('',(-10.0358241714444,64.97,13.1788877890042));
#37180=CARTESIAN_POINT('',(-10.1356594341564,64.97,13.7749103120746));
#37181=CARTESIAN_POINT('',(-10.1356594341564,64.97,13.7749103120746));
#37182=CARTESIAN_POINT('',(-10.192780409838,64.97,14.3959225765489));
#37183=CARTESIAN_POINT('',(-10.192780409838,64.97,14.3959225765489));
#37184=CARTESIAN_POINT('',(-10.208136822609,64.97,15.0386712143394));
#37185=CARTESIAN_POINT('',(-10.208136822609,64.97,15.0386712143394));
#37186=CARTESIAN_POINT('',(-10.1820769523934,64.97,15.7003835976467));
#37187=CARTESIAN_POINT('',(-10.1820769523934,64.97,15.7003835976467));
#37188=CARTESIAN_POINT('',(-10.1146191541229,64.97,16.3785524197668));
#37189=CARTESIAN_POINT('',(-10.1146191541229,64.97,16.3785524197668));
#37190=CARTESIAN_POINT('',(-9.87089260802485,64.97,16.5265840124582));
#37191=CARTESIAN_POINT('',(-9.87089260802485,64.97,16.5265840124582));
#37192=CARTESIAN_POINT('',(-9.625,64.97,16.6709890228504));
#37193=CARTESIAN_POINT('',(-9.625,64.97,16.6709890228504));
#37194=CARTESIAN_POINT('',(-9.37699528855417,64.97,16.8117357628067));
#37195=CARTESIAN_POINT('',(-9.37699528855417,64.97,16.8117357628067));
#37196=CARTESIAN_POINT('',(-9.12693289567172,64.97,16.9487933469585));
#37197=CARTESIAN_POINT('',(-9.12693289567172,64.97,16.9487933469585));
#37198=CARTESIAN_POINT('',(-8.50589256852586,64.97,16.6681291028841));
#37199=CARTESIAN_POINT('',(-8.50589256852586,64.97,16.6681291028841));
#37200=CARTESIAN_POINT('',(-7.91980289947517,64.97,16.3598414208564));
#37201=CARTESIAN_POINT('',(-7.91980289947517,64.97,16.3598414208564));
#37202=CARTESIAN_POINT('',(-7.37084445728621,64.97,16.0251680583905));
#37203=CARTESIAN_POINT('',(-7.37084445728621,64.97,16.0251680583905));
#37204=CARTESIAN_POINT('',(-6.86159254803068,64.97,15.6651937101241));
#37205=CARTESIAN_POINT('',(-6.86159254803068,64.97,15.6651937101241));
#37206=CARTESIAN_POINT('',(-6.39533953317997,64.97,15.2807225748869));
#37207=CARTESIAN_POINT('',(-5.13336928983991,64.97,12.0498844378435));
#37208=CARTESIAN_POINT('',(-3.13286772814965,64.97,6.80744119622516));
#37209=CARTESIAN_POINT('',(-3.38082377665168,64.97,12.617406105901));
#37210=CARTESIAN_POINT('',(-3.38082377665168,64.97,12.617406105901));
#37211=CARTESIAN_POINT('',(-1.57931400691349,64.97,13.0021906807592));
#37212=CARTESIAN_POINT('',(-2.0689307051291,64.97,12.8976134221558));
#37213=CARTESIAN_POINT('',(-2.11935175385489,64.97,16.3687597379803));
#37214=CARTESIAN_POINT('',(-0.540776800520307,64.97,6.52800023089147));
#37215=CARTESIAN_POINT('',(-2.10183478588267,64.97,16.4311637046244));
#37216=CARTESIAN_POINT('',(-2.10183478588267,64.97,16.4311637046244));
#37217=CARTESIAN_POINT('',(-1.8902833980495,64.97,16.997251982187));
#37218=CARTESIAN_POINT('',(-1.8902833980495,64.97,16.997251982187));
#37219=CARTESIAN_POINT('',(-1.62924548184168,64.97,17.5636248671243));
#37220=CARTESIAN_POINT('',(-1.62924548184168,64.97,17.5636248671243));
#37221=CARTESIAN_POINT('',(-1.32117020651705,64.97,18.1279397220841));
#37222=CARTESIAN_POINT('',(-1.32117020651705,64.97,18.1279397220842));
#37223=CARTESIAN_POINT('',(-0.967745505237382,64.97,18.6879695209193));
#37224=CARTESIAN_POINT('',(-0.967745505237382,64.97,18.6879695209193));
#37225=CARTESIAN_POINT('',(-0.57024092719168,64.97,19.2415520497946));
#37226=CARTESIAN_POINT('',(-0.57024092719168,64.97,19.2415520497946));
#37227=CARTESIAN_POINT('',(-0.285151750348432,64.97,19.247887896579));
#37228=CARTESIAN_POINT('',(-0.285151750348432,64.97,19.247887896579));
#37229=CARTESIAN_POINT('',(1.11022302462516E-15,64.97,19.25));
#37230=CARTESIAN_POINT('',(1.17872254417933E-15,64.97,19.25));
#37231=CARTESIAN_POINT('',(0.285151750348434,64.97,19.247887896579));
#37232=CARTESIAN_POINT('',(0.285151750348434,64.97,19.247887896579));
#37233=CARTESIAN_POINT('',(0.570240927191682,64.97,19.2415520497946));
#37234=CARTESIAN_POINT('',(0.570240927191682,64.97,19.2415520497946));
#37235=CARTESIAN_POINT('',(0.967745505237384,64.97,18.6879695209193));
#37236=CARTESIAN_POINT('',(0.967745505237385,64.97,18.6879695209193));
#37237=CARTESIAN_POINT('',(1.32117020651705,64.97,18.1279397220841));
#37238=CARTESIAN_POINT('',(1.32117020651705,64.97,18.1279397220842));
#37239=CARTESIAN_POINT('',(1.62924548184168,64.97,17.5636248671243));
#37240=CARTESIAN_POINT('',(1.62924548184168,64.97,17.5636248671243));
#37241=CARTESIAN_POINT('',(1.8902833980495,64.97,16.997251982187));
#37242=CARTESIAN_POINT('',(1.8902833980495,64.97,16.997251982187));
#37243=CARTESIAN_POINT('',(2.10183478588268,64.97,16.4311637046244));
#37244=CARTESIAN_POINT('',(1.57931400691349,64.97,13.0021906807592));
#37245=CARTESIAN_POINT('',(0.690577558838536,64.97,7.46185087477454));
#37246=CARTESIAN_POINT('',(3.38082377665168,64.97,12.617406105901));
#37247=CARTESIAN_POINT('',(3.38082377665168,64.97,12.617406105901));
#37248=CARTESIAN_POINT('',(5.13336928983992,64.97,12.0498844378435));
#37249=CARTESIAN_POINT('',(4.65706016176646,64.97,12.2041262243426));
#37250=CARTESIAN_POINT('',(6.34896741059669,64.97,15.2354376384623));
#37251=CARTESIAN_POINT('',(2.79567366841787,64.97,5.92380243612285));
#37252=CARTESIAN_POINT('',(6.39533953317997,64.97,15.2807225748869));
#37253=CARTESIAN_POINT('',(6.39533953317997,64.97,15.2807225748869));
#37254=CARTESIAN_POINT('',(6.86159254803069,64.97,15.6651937101241));
#37255=CARTESIAN_POINT('',(6.86159254803069,64.97,15.6651937101241));
#37256=CARTESIAN_POINT('',(7.37084445728622,64.97,16.0251680583905));
#37257=CARTESIAN_POINT('',(7.37084445728622,64.97,16.0251680583905));
#37258=CARTESIAN_POINT('',(7.91980289947518,64.97,16.3598414208564));
#37259=CARTESIAN_POINT('',(7.91980289947518,64.97,16.3598414208564));
#37260=CARTESIAN_POINT('',(8.50589256852587,64.97,16.6681291028841));
#37261=CARTESIAN_POINT('',(8.50589256852587,64.97,16.6681291028841));
#37262=CARTESIAN_POINT('',(9.12693289567173,64.97,16.9487933469585));
#37263=CARTESIAN_POINT('',(9.12693289567173,64.97,16.9487933469585));
#37264=CARTESIAN_POINT('',(9.37699528855417,64.97,16.8117357628067));
#37265=CARTESIAN_POINT('',(9.37699528855417,64.97,16.8117357628067));
#37266=CARTESIAN_POINT('',(9.625,64.97,16.6709890228504));
#37267=CARTESIAN_POINT('',(9.625,64.97,16.6709890228504));
#37268=CARTESIAN_POINT('',(9.87089260802485,64.97,16.5265840124582));
#37269=CARTESIAN_POINT('',(9.87089260802485,64.97,16.5265840124582));
#37270=CARTESIAN_POINT('',(10.1146191541229,64.97,16.3785524197668));
#37271=CARTESIAN_POINT('',(10.1146191541229,64.97,16.3785524197668));
#37272=CARTESIAN_POINT('',(10.1820769523934,64.97,15.7003835976467));
#37273=CARTESIAN_POINT('',(10.1820769523934,64.97,15.7003835976467));
#37274=CARTESIAN_POINT('',(10.208136822609,64.97,15.0386712143394));
#37275=CARTESIAN_POINT('',(10.208136822609,64.97,15.0386712143394));
#37276=CARTESIAN_POINT('',(10.192780409838,64.97,14.3959225765489));
#37277=CARTESIAN_POINT('',(10.192780409838,64.97,14.3959225765489));
#37278=CARTESIAN_POINT('',(10.1356594341564,64.97,13.7749103120746));
#37279=CARTESIAN_POINT('',(10.1356594341564,64.97,13.7749103120746));
#37280=CARTESIAN_POINT('',(10.0358241714444,64.97,13.1788877890042));
#37281=CARTESIAN_POINT('',(7.86882139091926,64.97,10.47057043093));
#37282=CARTESIAN_POINT('',(4.32898314662489,64.97,6.11686363738663));
#37283=CARTESIAN_POINT('',(9.23658232924928,64.97,9.23658232924927));
#37284=CARTESIAN_POINT('',(9.23658232924928,64.97,9.23658232924928));
#37285=CARTESIAN_POINT('',(10.47057043093,64.97,7.86882139091926));
#37286=CARTESIAN_POINT('',(10.1351955192135,64.97,8.24055326038936));
#37287=CARTESIAN_POINT('',(13.1160858846074,64.97,10.0197923273836));
#37288=CARTESIAN_POINT('',(5.38302563560253,64.97,3.73232656247359));
#37289=CARTESIAN_POINT('',(13.1788877890042,64.97,10.0358241714444));
#37290=CARTESIAN_POINT('',(13.1788877890042,64.97,10.0358241714444));
#37291=CARTESIAN_POINT('',(13.7749103120746,64.97,10.1356594341564));
#37292=CARTESIAN_POINT('',(13.7749103120746,64.97,10.1356594341564));
#37293=CARTESIAN_POINT('',(14.3959225765489,64.97,10.192780409838));
#37294=CARTESIAN_POINT('',(14.3959225765489,64.97,10.192780409838));
#37295=CARTESIAN_POINT('',(15.0386712143394,64.97,10.208136822609));
#37296=CARTESIAN_POINT('',(15.0386712143394,64.97,10.208136822609));
#37297=CARTESIAN_POINT('',(15.7003835976467,64.97,10.1820769523934));
#37298=CARTESIAN_POINT('',(15.7003835976467,64.97,10.1820769523934));
#37299=CARTESIAN_POINT('',(16.3785524197668,64.97,10.1146191541229));
#37300=CARTESIAN_POINT('',(16.3785524197668,64.97,10.1146191541229));
#37301=CARTESIAN_POINT('',(16.5265840124582,64.97,9.87089260802485));
#37302=CARTESIAN_POINT('',(16.5265840124582,64.97,9.87089260802485));
#37303=CARTESIAN_POINT('',(16.6709890228504,64.97,9.625));
#37304=CARTESIAN_POINT('',(16.6709890228504,64.97,9.625));
#37305=CARTESIAN_POINT('',(16.8117357628067,64.97,9.37699528855417));
#37306=CARTESIAN_POINT('',(16.8117357628067,64.97,9.37699528855417));
#37307=CARTESIAN_POINT('',(16.9487933469585,64.97,9.12693289567172));
#37308=CARTESIAN_POINT('',(16.9487933469585,64.97,9.12693289567172));
#37309=CARTESIAN_POINT('',(16.6681291028841,64.97,8.50589256852586));
#37310=CARTESIAN_POINT('',(16.6681291028841,64.97,8.50589256852586));
#37311=CARTESIAN_POINT('',(16.3598414208564,64.97,7.91980289947518));
#37312=CARTESIAN_POINT('',(16.3598414208564,64.97,7.91980289947517));
#37313=CARTESIAN_POINT('',(16.0251680583905,64.97,7.37084445728621));
#37314=CARTESIAN_POINT('',(16.0251680583905,64.97,7.37084445728621));
#37315=CARTESIAN_POINT('',(15.6651937101241,64.97,6.86159254803069));
#37316=CARTESIAN_POINT('',(15.6651937101241,64.97,6.86159254803069));
#37317=CARTESIAN_POINT('',(15.2807225748869,64.97,6.39533953317997));
#37318=CARTESIAN_POINT('',(12.0498844378435,64.97,5.13336928983991));
#37319=CARTESIAN_POINT('',(6.80744119622516,64.97,3.13286772814966));
#37320=CARTESIAN_POINT('',(12.617406105901,64.97,3.38082377665168));
#37321=CARTESIAN_POINT('',(12.617406105901,64.97,3.38082377665168));
#37322=CARTESIAN_POINT('',(13.0021906807592,64.97,1.57931400691349));
#37323=CARTESIAN_POINT('',(12.8976134221558,64.97,2.0689307051291));
#37324=CARTESIAN_POINT('',(16.3687597379803,64.97,2.11935175385489));
#37325=CARTESIAN_POINT('',(6.52800023089146,64.97,0.540776800520309));
#37326=CARTESIAN_POINT('',(16.4311637046244,64.97,2.10183478588267));
#37327=CARTESIAN_POINT('',(16.4311637046244,64.97,2.10183478588267));
#37328=CARTESIAN_POINT('',(16.997251982187,64.97,1.8902833980495));
#37329=CARTESIAN_POINT('',(16.997251982187,64.97,1.8902833980495));
#37330=CARTESIAN_POINT('',(17.5636248671243,64.97,1.62924548184168));
#37331=CARTESIAN_POINT('',(17.5636248671243,64.97,1.62924548184168));
#37332=CARTESIAN_POINT('',(18.1279397220841,64.97,1.32117020651705));
#37333=CARTESIAN_POINT('',(18.1279397220842,64.97,1.32117020651705));
#37334=CARTESIAN_POINT('',(18.6879695209193,64.97,0.967745505237385));
#37335=CARTESIAN_POINT('',(18.6879695209193,64.97,0.967745505237384));
#37336=CARTESIAN_POINT('',(19.2415520497946,64.97,0.570240927191681));
#37337=CARTESIAN_POINT('',(19.2415520497946,64.97,0.570240927191682));
#37338=CARTESIAN_POINT('',(19.247887896579,64.97,0.285151750348434));
#37339=CARTESIAN_POINT('',(19.247887896579,64.97,0.285151750348434));
#37340=CARTESIAN_POINT('',(19.25,64.97,0.));
#37341=CARTESIAN_POINT('',(19.25,64.97,0.));
#37342=CARTESIAN_POINT('',(19.247887896579,64.97,-0.285151750348434));
#37343=CARTESIAN_POINT('',(19.247887896579,64.97,-0.285151750348434));
#37344=CARTESIAN_POINT('',(19.2415520497946,64.97,-0.570240927191681));
#37345=CARTESIAN_POINT('',(19.2415520497946,64.97,-0.570240927191682));
#37346=CARTESIAN_POINT('',(18.6879695209193,64.97,-0.967745505237385));
#37347=CARTESIAN_POINT('',(18.6879695209193,64.97,-0.967745505237384));
#37348=CARTESIAN_POINT('',(18.1279397220841,64.97,-1.32117020651705));
#37349=CARTESIAN_POINT('',(18.1279397220842,64.97,-1.32117020651705));
#37350=CARTESIAN_POINT('',(17.5636248671243,64.97,-1.62924548184168));
#37351=CARTESIAN_POINT('',(17.5636248671243,64.97,-1.62924548184168));
#37352=CARTESIAN_POINT('',(16.997251982187,64.97,-1.8902833980495));
#37353=CARTESIAN_POINT('',(16.997251982187,64.97,-1.8902833980495));
#37354=CARTESIAN_POINT('',(16.4311637046244,64.97,-2.10183478588267));
#37355=CARTESIAN_POINT('',(13.0021906807592,64.97,-1.57931400691349));
#37356=CARTESIAN_POINT('',(7.46185087477454,64.97,-0.690577558838536));
#37357=CARTESIAN_POINT('',(12.617406105901,64.97,-3.38082377665168));
#37358=CARTESIAN_POINT('',(12.617406105901,64.97,-3.38082377665168));
#37359=CARTESIAN_POINT('',(12.0498844378435,64.97,-5.13336928983991));
#37360=CARTESIAN_POINT('',(12.2041262243426,64.97,-4.65706016176646));
#37361=CARTESIAN_POINT('',(15.2354376384623,64.97,-6.34896741059669));
#37362=CARTESIAN_POINT('',(5.92380243612284,64.97,-2.79567366841787));
#37363=CARTESIAN_POINT('',(15.2807225748869,64.97,-6.39533953317997));
#37364=CARTESIAN_POINT('',(15.2807225748869,64.97,-6.39533953317997));
#37365=CARTESIAN_POINT('',(15.6651937101241,64.97,-6.86159254803069));
#37366=CARTESIAN_POINT('',(15.6651937101241,64.97,-6.86159254803069));
#37367=CARTESIAN_POINT('',(16.0251680583905,64.97,-7.37084445728621));
#37368=CARTESIAN_POINT('',(16.0251680583905,64.97,-7.37084445728621));
#37369=CARTESIAN_POINT('',(16.3598414208564,64.97,-7.91980289947517));
#37370=CARTESIAN_POINT('',(16.3598414208564,64.97,-7.91980289947517));
#37371=CARTESIAN_POINT('',(16.6681291028841,64.97,-8.50589256852586));
#37372=CARTESIAN_POINT('',(16.6681291028841,64.97,-8.50589256852586));
#37373=CARTESIAN_POINT('',(16.9487933469585,64.97,-9.12693289567172));
#37374=CARTESIAN_POINT('',(16.9487933469585,64.97,-9.12693289567172));
#37375=CARTESIAN_POINT('',(16.8117357628067,64.97,-9.37699528855417));
#37376=CARTESIAN_POINT('',(16.8117357628067,64.97,-9.37699528855417));
#37377=CARTESIAN_POINT('',(16.6709890228504,64.97,-9.625));
#37378=CARTESIAN_POINT('',(16.6709890228504,64.97,-9.625));
#37379=CARTESIAN_POINT('',(16.5265840124582,64.97,-9.87089260802485));
#37380=CARTESIAN_POINT('',(16.5265840124582,64.97,-9.87089260802485));
#37381=CARTESIAN_POINT('',(16.3785524197668,64.97,-10.1146191541229));
#37382=CARTESIAN_POINT('',(16.3785524197668,64.97,-10.1146191541229));
#37383=CARTESIAN_POINT('',(15.7003835976467,64.97,-10.1820769523934));
#37384=CARTESIAN_POINT('',(15.7003835976467,64.97,-10.1820769523934));
#37385=CARTESIAN_POINT('',(15.0386712143394,64.97,-10.208136822609));
#37386=CARTESIAN_POINT('',(15.0386712143394,64.97,-10.208136822609));
#37387=CARTESIAN_POINT('',(14.3959225765489,64.97,-10.192780409838));
#37388=CARTESIAN_POINT('',(14.3959225765489,64.97,-10.192780409838));
#37389=CARTESIAN_POINT('',(13.7749103120746,64.97,-10.1356594341564));
#37390=CARTESIAN_POINT('',(13.7749103120746,64.97,-10.1356594341564));
#37391=CARTESIAN_POINT('',(13.1788877890042,64.97,-10.0358241714444));
#37392=CARTESIAN_POINT('',(10.47057043093,64.97,-7.86882139091926));
#37393=CARTESIAN_POINT('',(6.11686363738662,64.97,-4.32898314662489));
#37394=CARTESIAN_POINT('',(9.23658232924928,64.97,-9.23658232924928));
#37395=CARTESIAN_POINT('',(9.23658232924928,64.97,-9.23658232924928));
#37396=CARTESIAN_POINT('',(7.86882139091926,64.97,-10.47057043093));
#37397=CARTESIAN_POINT('',(8.24055326038937,64.97,-10.1351955192135));
#37398=CARTESIAN_POINT('',(10.0197923273836,64.97,-13.1160858846074));
#37399=CARTESIAN_POINT('',(3.73232656247359,64.97,-5.38302563560254));
#37400=CARTESIAN_POINT('',(10.0358241714444,64.97,-13.1788877890042));
#37401=CARTESIAN_POINT('',(10.0358241714444,64.97,-13.1788877890042));
#37402=CARTESIAN_POINT('',(10.1356594341564,64.97,-13.7749103120746));
#37403=CARTESIAN_POINT('',(10.1356594341564,64.97,-13.7749103120746));
#37404=CARTESIAN_POINT('',(10.192780409838,64.97,-14.3959225765489));
#37405=CARTESIAN_POINT('',(10.192780409838,64.97,-14.3959225765489));
#37406=CARTESIAN_POINT('',(10.208136822609,64.97,-15.0386712143394));
#37407=CARTESIAN_POINT('',(10.208136822609,64.97,-15.0386712143394));
#37408=CARTESIAN_POINT('',(10.1820769523934,64.97,-15.7003835976467));
#37409=CARTESIAN_POINT('',(10.1820769523934,64.97,-15.7003835976467));
#37410=CARTESIAN_POINT('',(10.1146191541229,64.97,-16.3785524197668));
#37411=CARTESIAN_POINT('',(10.1146191541229,64.97,-16.3785524197668));
#37412=CARTESIAN_POINT('',(9.87089260802485,64.97,-16.5265840124582));
#37413=CARTESIAN_POINT('',(9.87089260802485,64.97,-16.5265840124582));
#37414=CARTESIAN_POINT('',(9.625,64.97,-16.6709890228504));
#37415=CARTESIAN_POINT('',(9.625,64.97,-16.6709890228504));
#37416=CARTESIAN_POINT('',(9.37699528855417,64.97,-16.8117357628067));
#37417=CARTESIAN_POINT('',(9.37699528855417,64.97,-16.8117357628067));
#37418=CARTESIAN_POINT('',(9.12693289567173,64.97,-16.9487933469585));
#37419=CARTESIAN_POINT('',(9.12693289567173,64.97,-16.9487933469585));
#37420=CARTESIAN_POINT('',(8.50589256852587,64.97,-16.6681291028841));
#37421=CARTESIAN_POINT('',(8.50589256852587,64.97,-16.6681291028841));
#37422=CARTESIAN_POINT('',(7.91980289947518,64.97,-16.3598414208564));
#37423=CARTESIAN_POINT('',(7.91980289947518,64.97,-16.3598414208564));
#37424=CARTESIAN_POINT('',(7.37084445728622,64.97,-16.0251680583905));
#37425=CARTESIAN_POINT('',(7.37084445728622,64.97,-16.0251680583905));
#37426=CARTESIAN_POINT('',(6.86159254803069,64.97,-15.6651937101241));
#37427=CARTESIAN_POINT('',(6.86159254803069,64.97,-15.6651937101241));
#37428=CARTESIAN_POINT('',(6.39533953317997,64.97,-15.2807225748869));
#37429=CARTESIAN_POINT('',(5.13336928983992,64.97,-12.0498844378435));
#37430=CARTESIAN_POINT('',(3.13286772814966,64.97,-6.80744119622516));
#37431=CARTESIAN_POINT('',(3.38082377665168,64.97,-12.617406105901));
#37432=CARTESIAN_POINT('',(3.38082377665168,64.97,-12.617406105901));
#37433=CARTESIAN_POINT('',(1.57931400691349,64.97,-13.0021906807592));
#37434=CARTESIAN_POINT('',(2.0689307051291,64.97,-12.8976134221558));
#37435=CARTESIAN_POINT('',(2.11935175385489,64.97,-16.3687597379803));
#37436=CARTESIAN_POINT('',(0.540776800520309,64.97,-6.52800023089146));
#37437=CARTESIAN_POINT('',(2.10183478588268,64.97,-16.4311637046244));
#37438=CARTESIAN_POINT('',(2.10183478588268,64.97,-16.4311637046244));
#37439=CARTESIAN_POINT('',(1.8902833980495,64.97,-16.997251982187));
#37440=CARTESIAN_POINT('',(1.8902833980495,64.97,-16.997251982187));
#37441=CARTESIAN_POINT('',(1.62924548184168,64.97,-17.5636248671243));
#37442=CARTESIAN_POINT('',(1.62924548184168,64.97,-17.5636248671243));
#37443=CARTESIAN_POINT('',(1.32117020651705,64.97,-18.1279397220842));
#37444=CARTESIAN_POINT('',(1.32117020651705,64.97,-18.1279397220842));
#37445=CARTESIAN_POINT('',(0.967745505237384,64.97,-18.6879695209193));
#37446=CARTESIAN_POINT('',(0.967745505237385,64.97,-18.6879695209193));
#37447=CARTESIAN_POINT('',(0.570240927191682,64.97,-19.2415520497946));
#37448=CARTESIAN_POINT('',(0.570240927191682,64.97,-19.2415520497946));
#37449=CARTESIAN_POINT('',(0.285151750348434,64.97,-19.247887896579));
#37450=CARTESIAN_POINT('',(0.285151750348434,64.97,-19.247887896579));
#37451=CARTESIAN_POINT('',(1.11022302462516E-15,64.97,-19.25));
#37452=CARTESIAN_POINT('',(1.17872254417933E-15,64.97,-19.25));
#37453=CARTESIAN_POINT('',(-0.285151750348432,64.97,-19.247887896579));
#37454=CARTESIAN_POINT('',(-0.285151750348432,64.97,-19.247887896579));
#37455=CARTESIAN_POINT('',(-0.57024092719168,64.97,-19.2415520497946));
#37456=CARTESIAN_POINT('',(-0.57024092719168,64.97,-19.2415520497946));
#37457=CARTESIAN_POINT('',(-0.967745505237382,64.97,-18.6879695209193));
#37458=CARTESIAN_POINT('',(-0.967745505237382,64.97,-18.6879695209193));
#37459=CARTESIAN_POINT('',(-1.32117020651705,64.97,-18.1279397220842));
#37460=CARTESIAN_POINT('',(-1.32117020651705,64.97,-18.1279397220842));
#37461=CARTESIAN_POINT('',(-1.62924548184168,64.97,-17.5636248671243));
#37462=CARTESIAN_POINT('',(-1.62924548184168,64.97,-17.5636248671243));
#37463=CARTESIAN_POINT('',(-1.8902833980495,64.97,-16.997251982187));
#37464=CARTESIAN_POINT('',(-1.8902833980495,64.97,-16.997251982187));
#37465=CARTESIAN_POINT('',(-2.10183478588267,64.97,-16.4311637046244));
#37466=CARTESIAN_POINT('',(-1.04094977927525E-15,64.97,-8.5));
#37467=CARTESIAN_POINT('Origin',(0.,64.97,0.));
#37468=CARTESIAN_POINT('Origin',(0.78762107654243,64.72,-6.48840347098469));
#37469=CARTESIAN_POINT('',(2.25993461117485,64.7518675845618,-15.8679351687486));
#37470=CARTESIAN_POINT('',(4.58946667393372,61.1372984587275,-7.56900801586535));
#37471=CARTESIAN_POINT('',(9.06586927392218,57.3246773483287,-11.4031369126593));
#37472=CARTESIAN_POINT('',(3.70127502843353,62.0175738804576,-7.58981354975406));
#37473=CARTESIAN_POINT('Origin',(2.89929593438233,64.72,-6.8965715342494));
#37474=CARTESIAN_POINT('',(5.33144828123002,64.47,-13.9714037445473));
#37475=CARTESIAN_POINT('',(2.40887949353887,63.4588711803305,-9.14872003481927));
#37476=CARTESIAN_POINT('',(4.65706016176646,64.47,-12.2041262243426));
#37477=CARTESIAN_POINT('',(2.66572414061501,64.47,-6.98570187227364));
#37478=CARTESIAN_POINT('',(-1.81865838957184,57.6721893244721,-14.3011391500957));
#37479=CARTESIAN_POINT('Origin',(3.92630159633414,64.72,-5.22531169760465));
#37480=CARTESIAN_POINT('',(9.89112836854343,64.7518675845618,-12.6120676561534));
#37481=CARTESIAN_POINT('',(7.75909873738132,61.1372984587275,-4.26021988622061));
#37482=CARTESIAN_POINT('',(13.5528415549351,57.3246773483287,-5.34247161223395));
#37483=CARTESIAN_POINT('',(7.00030497589346,62.0175738804575,-4.72233382985757));
#37484=CARTESIAN_POINT('Origin',(5.95914969938874,64.72,-4.52295818048544));
#37485=CARTESIAN_POINT('',(11.6028715227817,64.47,-9.43386642869196));
#37486=CARTESIAN_POINT('',(6.66051085346965,63.4588711803305,-6.71858421549571));
#37487=CARTESIAN_POINT('',(10.1351955192135,64.47,-8.24055326038936));
#37488=CARTESIAN_POINT('',(5.80143576139085,64.47,-4.71693321434598));
#37489=CARTESIAN_POINT('',(5.57556520887294,57.6721893244721,-13.294479001825));
#37490=CARTESIAN_POINT('Origin',(6.01293277414708,64.72,-2.56210187465055));
#37491=CARTESIAN_POINT('',(14.8720022673282,64.7518675845618,-5.97680680020517));
#37492=CARTESIAN_POINT('',(8.84968656015429,61.1372984587275,0.190090721515985));
#37493=CARTESIAN_POINT('',(14.4083408861561,57.3246773483287,2.14970464227572));
#37494=CARTESIAN_POINT('',(8.42360885829113,62.0175738804575,-0.589508573860589));
#37495=CARTESIAN_POINT('Origin',(7.42225411486777,64.72,-0.937421834860657));
#37496=CARTESIAN_POINT('',(14.765314709922,64.47,-2.36853222176556));
#37497=CARTESIAN_POINT('',(9.12746370903452,63.4588711803305,-2.48820918134962));
#37498=CARTESIAN_POINT('',(12.8976134221558,64.47,-2.0689307051291));
#37499=CARTESIAN_POINT('',(7.38265735496099,64.47,-1.18426611088278));
#37500=CARTESIAN_POINT('',(11.4758206122532,57.6721893244721,-8.72557394122277));
#37501=CARTESIAN_POINT('Origin',(6.48840347098469,64.72,0.78762107654243));
#37502=CARTESIAN_POINT('',(15.8679351687486,64.7518675845618,2.25993461117485));
#37503=CARTESIAN_POINT('',(7.56900801586535,61.1372984587275,4.58946667393373));
#37504=CARTESIAN_POINT('',(11.4031369126593,57.3246773483287,9.06586927392218));
#37505=CARTESIAN_POINT('',(7.58981354975407,62.0175738804576,3.70127502843351));
#37506=CARTESIAN_POINT('Origin',(6.8965715342494,64.72,2.89929593438233));
#37507=CARTESIAN_POINT('',(13.9714037445473,64.47,5.33144828123002));
#37508=CARTESIAN_POINT('',(9.14872003481924,63.4588711803305,2.40887949353882));
#37509=CARTESIAN_POINT('',(12.2041262243426,64.47,4.65706016176646));
#37510=CARTESIAN_POINT('',(6.98570187227364,64.47,2.66572414061501));
#37511=CARTESIAN_POINT('',(14.3011391500957,57.6721893244721,-1.81865838957184));
#37512=CARTESIAN_POINT('Origin',(5.22531169760465,64.72,3.92630159633414));
#37513=CARTESIAN_POINT('',(12.6120676561534,64.7518675845618,9.89112836854343));
#37514=CARTESIAN_POINT('',(4.26021988622058,61.1372984587275,7.75909873738136));
#37515=CARTESIAN_POINT('',(5.34247161223395,57.3246773483287,13.5528415549351));
#37516=CARTESIAN_POINT('',(4.7223338298576,62.0175738804576,7.00030497589344));
#37517=CARTESIAN_POINT('Origin',(4.52295818048543,64.72,5.95914969938874));
#37518=CARTESIAN_POINT('',(9.43386642869196,64.47,11.6028715227817));
#37519=CARTESIAN_POINT('',(6.71858421549571,63.4588711803305,6.66051085346967));
#37520=CARTESIAN_POINT('',(8.24055326038937,64.47,10.1351955192135));
#37521=CARTESIAN_POINT('',(4.71693321434598,64.47,5.80143576139086));
#37522=CARTESIAN_POINT('',(13.294479001825,57.6721893244721,5.57556520887294));
#37523=CARTESIAN_POINT('Origin',(2.56210187465055,64.72,6.01293277414708));
#37524=CARTESIAN_POINT('',(5.97680680020517,64.7518675845618,14.8720022673282));
#37525=CARTESIAN_POINT('',(-0.19009072151597,61.1372984587275,8.84968656015429));
#37526=CARTESIAN_POINT('',(-2.14970464227572,57.3246773483287,14.4083408861561));
#37527=CARTESIAN_POINT('',(0.589508573860579,62.0175738804575,8.42360885829113));
#37528=CARTESIAN_POINT('Origin',(0.937421834860657,64.72,7.42225411486777));
#37529=CARTESIAN_POINT('',(2.36853222176556,64.47,14.765314709922));
#37530=CARTESIAN_POINT('',(2.4882091813496,63.4588711803305,9.12746370903455));
#37531=CARTESIAN_POINT('',(2.0689307051291,64.47,12.8976134221558));
#37532=CARTESIAN_POINT('',(1.18426611088278,64.47,7.38265735496099));
#37533=CARTESIAN_POINT('',(8.72557394122277,57.6721893244721,11.4758206122532));
#37534=CARTESIAN_POINT('Origin',(-0.787621076542428,64.72,6.48840347098469));
#37535=CARTESIAN_POINT('',(-2.25993461117485,64.7518675845618,15.8679351687486));
#37536=CARTESIAN_POINT('',(-4.58946667393372,61.1372984587275,7.56900801586535));
#37537=CARTESIAN_POINT('',(-9.06586927392218,57.3246773483287,11.4031369126593));
#37538=CARTESIAN_POINT('',(-3.70127502843353,62.0175738804576,7.58981354975406));
#37539=CARTESIAN_POINT('Origin',(-2.89929593438233,64.72,6.8965715342494));
#37540=CARTESIAN_POINT('',(-5.33144828123002,64.47,13.9714037445473));
#37541=CARTESIAN_POINT('',(-2.40887949353884,63.4588711803305,9.14872003481926));
#37542=CARTESIAN_POINT('',(-4.65706016176645,64.47,12.2041262243426));
#37543=CARTESIAN_POINT('',(-2.66572414061501,64.47,6.98570187227364));
#37544=CARTESIAN_POINT('',(1.81865838957184,57.6721893244721,14.3011391500957));
#37545=CARTESIAN_POINT('Origin',(-3.92630159633414,64.72,5.22531169760465));
#37546=CARTESIAN_POINT('',(-9.89112836854343,64.7518675845618,12.6120676561534));
#37547=CARTESIAN_POINT('',(-7.75909873738135,61.1372984587275,4.26021988622059));
#37548=CARTESIAN_POINT('',(-13.5528415549351,57.3246773483287,5.34247161223395));
#37549=CARTESIAN_POINT('',(-7.0003049758934,62.0175738804576,4.72233382985765));
#37550=CARTESIAN_POINT('Origin',(-5.95914969938874,64.72,4.52295818048543));
#37551=CARTESIAN_POINT('',(-11.6028715227817,64.47,9.43386642869196));
#37552=CARTESIAN_POINT('',(-6.66051085346952,63.4588711803304,6.71858421549571));
#37553=CARTESIAN_POINT('',(-10.1351955192135,64.47,8.24055326038937));
#37554=CARTESIAN_POINT('',(-5.80143576139086,64.47,4.71693321434598));
#37555=CARTESIAN_POINT('',(-5.57556520887294,57.6721893244721,13.294479001825));
#37556=CARTESIAN_POINT('Origin',(-6.01293277414708,64.72,2.56210187465055));
#37557=CARTESIAN_POINT('',(-14.8720022673282,64.7518675845618,5.97680680020517));
#37558=CARTESIAN_POINT('',(-8.84968656015429,61.1372984587275,-0.190090721515974));
#37559=CARTESIAN_POINT('',(-14.4083408861561,57.3246773483287,-2.14970464227572));
#37560=CARTESIAN_POINT('',(-8.42360885829112,62.0175738804576,0.589508573860645));
#37561=CARTESIAN_POINT('Origin',(-7.42225411486777,64.72,0.937421834860659));
#37562=CARTESIAN_POINT('',(-14.765314709922,64.47,2.36853222176556));
#37563=CARTESIAN_POINT('',(-9.12746370903443,63.4588711803304,2.48820918134967));
#37564=CARTESIAN_POINT('',(-12.8976134221558,64.47,2.0689307051291));
#37565=CARTESIAN_POINT('',(-7.38265735496099,64.47,1.18426611088278));
#37566=CARTESIAN_POINT('',(-11.4758206122532,57.6721893244721,8.72557394122277));
#37567=CARTESIAN_POINT('Origin',(-6.48840347098469,64.72,-0.787621076542431));
#37568=CARTESIAN_POINT('',(-15.8679351687486,64.7518675845618,-2.25993461117485));
#37569=CARTESIAN_POINT('',(-7.56900801586535,61.1372984587275,-4.58946667393371));
#37570=CARTESIAN_POINT('',(-11.4031369126593,57.3246773483287,-9.06586927392218));
#37571=CARTESIAN_POINT('',(-7.58981354975408,62.0175738804576,-3.70127502843348));
#37572=CARTESIAN_POINT('Origin',(-6.8965715342494,64.72,-2.89929593438234));
#37573=CARTESIAN_POINT('',(-13.9714037445473,64.47,-5.33144828123002));
#37574=CARTESIAN_POINT('',(-9.14872003481919,63.4588711803304,-2.40887949353873));
#37575=CARTESIAN_POINT('',(-12.2041262243426,64.47,-4.65706016176646));
#37576=CARTESIAN_POINT('',(-6.98570187227364,64.47,-2.66572414061501));
#37577=CARTESIAN_POINT('',(-14.3011391500957,57.6721893244721,1.81865838957184));
#37578=CARTESIAN_POINT('Origin',(-5.22531169760465,64.72,-3.92630159633413));
#37579=CARTESIAN_POINT('',(-12.6120676561534,64.7518675845618,-9.89112836854343));
#37580=CARTESIAN_POINT('',(-4.26021988622061,61.1372984587275,-7.75909873738132));
#37581=CARTESIAN_POINT('',(-5.34247161223396,57.3246773483287,-13.5528415549351));
#37582=CARTESIAN_POINT('',(-4.72233382985763,62.0175738804576,-7.00030497589342));
#37583=CARTESIAN_POINT('Origin',(-4.52295818048544,64.72,-5.95914969938874));
#37584=CARTESIAN_POINT('',(-9.43386642869197,64.47,-11.6028715227817));
#37585=CARTESIAN_POINT('',(-6.71858421549571,63.4588711803305,-6.66051085346966));
#37586=CARTESIAN_POINT('',(-8.24055326038937,64.47,-10.1351955192135));
#37587=CARTESIAN_POINT('',(-4.71693321434598,64.47,-5.80143576139086));
#37588=CARTESIAN_POINT('',(-13.294479001825,57.6721893244721,-5.57556520887294));
#37589=CARTESIAN_POINT('Origin',(-2.56210187465055,64.72,-6.01293277414708));
#37590=CARTESIAN_POINT('',(-5.97680680020517,64.7518675845618,-14.8720022673282));
#37591=CARTESIAN_POINT('',(0.190090721516171,61.1372984587273,-8.84968656015439));
#37592=CARTESIAN_POINT('',(2.14970464227572,57.3246773483287,-14.4083408861561));
#37593=CARTESIAN_POINT('',(-0.589508573860655,62.0175738804576,-8.42360885829113));
#37594=CARTESIAN_POINT('Origin',(2.,-35.,7.94));
#37595=CARTESIAN_POINT('',(2.,-35.,7.68398334199131));
#37596=CARTESIAN_POINT('',(-2.,-35.,7.68398334199131));
#37597=CARTESIAN_POINT('Origin',(0.,-35.,0.));
#37598=CARTESIAN_POINT('',(2.,-35.,5.94));
#37599=CARTESIAN_POINT('',(2.,-35.,7.94));
#37600=CARTESIAN_POINT('',(-2.,-35.,5.94));
#37601=CARTESIAN_POINT('',(-2.,-35.,5.94));
#37602=CARTESIAN_POINT('',(-2.,-35.,7.94));
#37603=CARTESIAN_POINT('Origin',(-2.,-35.,7.94));
#37604=CARTESIAN_POINT('',(-2.,-10.,7.68398334199131));
#37605=CARTESIAN_POINT('',(-2.,-9.62499999999999,7.68398334199131));
#37606=CARTESIAN_POINT('',(-2.,-10.,5.94));
#37607=CARTESIAN_POINT('',(-2.,-10.,5.94));
#37608=CARTESIAN_POINT('',(-2.,-10.,7.94));
#37609=CARTESIAN_POINT('Origin',(2.,-10.,7.94));
#37610=CARTESIAN_POINT('',(2.,-10.,7.68398334199131));
#37611=CARTESIAN_POINT('',(2.,-9.62499999999999,7.68398334199131));
#37612=CARTESIAN_POINT('',(2.,-10.,5.94));
#37613=CARTESIAN_POINT('',(2.,-10.,7.94));
#37614=CARTESIAN_POINT('',(2.,-35.,5.94));
#37615=CARTESIAN_POINT('Origin',(-2.,-10.,7.94));
#37616=CARTESIAN_POINT('Origin',(0.,-10.,0.));
#37617=CARTESIAN_POINT('',(2.,-10.,5.94));
#37618=CARTESIAN_POINT('Origin',(0.,-22.5,5.94));
#37619=CARTESIAN_POINT('Origin',(-2.0689307051291,37.03,-12.8976134221558));
#37620=CARTESIAN_POINT('',(-3.38082377665168,37.03,-12.617406105901));
#37621=CARTESIAN_POINT('',(-2.0689307051291,37.03,-12.8976134221558));
#37622=CARTESIAN_POINT('Origin',(-2.36853222176555,37.03,-14.765314709922));
#37623=CARTESIAN_POINT('',(-2.36853222176555,37.03,-14.765314709922));
#37624=CARTESIAN_POINT('Origin',(-2.35695480224783,37.03,-15.3107143126737));
#37625=CARTESIAN_POINT('Origin',(-1.8902833980495,37.03,-16.997251982187));
#37626=CARTESIAN_POINT('',(-1.8902833980495,37.03,-16.997251982187));
#37627=CARTESIAN_POINT('Origin',(-1.62924548184168,37.03,-17.5636248671243));
#37628=CARTESIAN_POINT('',(-1.62924548184168,37.03,-17.5636248671243));
#37629=CARTESIAN_POINT('Origin',(-1.32117020651705,37.03,-18.1279397220842));
#37630=CARTESIAN_POINT('',(-1.32117020651705,37.03,-18.1279397220842));
#37631=CARTESIAN_POINT('Origin',(-0.967745505237382,37.03,-18.6879695209193));
#37632=CARTESIAN_POINT('',(-0.967745505237382,37.03,-18.6879695209193));
#37633=CARTESIAN_POINT('Origin',(-0.57024092719168,37.03,-19.2415520497946));
#37634=CARTESIAN_POINT('',(-0.57024092719168,37.03,-19.2415520497946));
#37635=CARTESIAN_POINT('Origin',(-0.285151750348432,37.03,-19.247887896579));
#37636=CARTESIAN_POINT('',(-0.285151750348432,37.03,-19.247887896579));
#37637=CARTESIAN_POINT('Origin',(1.17961196366423E-15,37.03,-19.25));
#37638=CARTESIAN_POINT('',(1.17872254417933E-15,37.03,-19.25));
#37639=CARTESIAN_POINT('Origin',(0.285151750348434,37.03,-19.247887896579));
#37640=CARTESIAN_POINT('',(0.285151750348434,37.03,-19.247887896579));
#37641=CARTESIAN_POINT('Origin',(0.570240927191682,37.03,-19.2415520497946));
#37642=CARTESIAN_POINT('',(0.570240927191682,37.03,-19.2415520497946));
#37643=CARTESIAN_POINT('Origin',(0.967745505237385,37.03,-18.6879695209193));
#37644=CARTESIAN_POINT('',(0.967745505237385,37.03,-18.6879695209193));
#37645=CARTESIAN_POINT('Origin',(1.32117020651705,37.03,-18.1279397220842));
#37646=CARTESIAN_POINT('',(1.32117020651705,37.03,-18.1279397220842));
#37647=CARTESIAN_POINT('Origin',(1.62924548184168,37.03,-17.5636248671243));
#37648=CARTESIAN_POINT('',(1.62924548184168,37.03,-17.5636248671243));
#37649=CARTESIAN_POINT('Origin',(1.8902833980495,37.03,-16.997251982187));
#37650=CARTESIAN_POINT('',(1.8902833980495,37.03,-16.997251982187));
#37651=CARTESIAN_POINT('Origin',(2.10183478588268,37.03,-16.4311637046244));
#37652=CARTESIAN_POINT('',(2.10183478588268,37.03,-16.4311637046244));
#37653=CARTESIAN_POINT('Origin',(2.25993461117485,37.03,-15.8679351687486));
#37654=CARTESIAN_POINT('',(2.25993461117485,37.03,-15.8679351687486));
#37655=CARTESIAN_POINT('Origin',(2.35695480224784,37.03,-15.3107143126737));
#37656=CARTESIAN_POINT('Origin',(3.38082377665168,37.03,-12.617406105901));
#37657=CARTESIAN_POINT('',(3.38082377665168,37.03,-12.617406105901));
#37658=CARTESIAN_POINT('Origin',(4.65706016176646,37.03,-12.2041262243426));
#37659=CARTESIAN_POINT('',(4.65706016176646,37.03,-12.2041262243426));
#37660=CARTESIAN_POINT('Origin',(5.33144828123002,37.03,-13.9714037445473));
#37661=CARTESIAN_POINT('',(5.33144828123002,37.03,-13.9714037445473));
#37662=CARTESIAN_POINT('Origin',(5.61417442201851,37.03,-14.4379449459854));
#37663=CARTESIAN_POINT('Origin',(6.86159254803069,37.03,-15.6651937101241));
#37664=CARTESIAN_POINT('',(6.86159254803069,37.03,-15.6651937101241));
#37665=CARTESIAN_POINT('Origin',(7.37084445728622,37.03,-16.0251680583905));
#37666=CARTESIAN_POINT('',(7.37084445728622,37.03,-16.0251680583905));
#37667=CARTESIAN_POINT('Origin',(7.91980289947518,37.03,-16.3598414208564));
#37668=CARTESIAN_POINT('',(7.91980289947518,37.03,-16.3598414208564));
#37669=CARTESIAN_POINT('Origin',(8.50589256852587,37.03,-16.6681291028841));
#37670=CARTESIAN_POINT('',(8.50589256852587,37.03,-16.6681291028841));
#37671=CARTESIAN_POINT('Origin',(9.12693289567173,37.03,-16.9487933469585));
#37672=CARTESIAN_POINT('',(9.12693289567173,37.03,-16.9487933469585));
#37673=CARTESIAN_POINT('Origin',(9.37699528855417,37.03,-16.8117357628067));
#37674=CARTESIAN_POINT('',(9.37699528855417,37.03,-16.8117357628067));
#37675=CARTESIAN_POINT('Origin',(9.625,37.03,-16.6709890228504));
#37676=CARTESIAN_POINT('',(9.625,37.03,-16.6709890228504));
#37677=CARTESIAN_POINT('Origin',(9.87089260802485,37.03,-16.5265840124582));
#37678=CARTESIAN_POINT('',(9.87089260802485,37.03,-16.5265840124582));
#37679=CARTESIAN_POINT('Origin',(10.1146191541229,37.03,-16.3785524197668));
#37680=CARTESIAN_POINT('',(10.1146191541229,37.03,-16.3785524197668));
#37681=CARTESIAN_POINT('Origin',(10.1820769523934,37.03,-15.7003835976467));
#37682=CARTESIAN_POINT('',(10.1820769523934,37.03,-15.7003835976467));
#37683=CARTESIAN_POINT('Origin',(10.208136822609,37.03,-15.0386712143394));
#37684=CARTESIAN_POINT('',(10.208136822609,37.03,-15.0386712143394));
#37685=CARTESIAN_POINT('Origin',(10.192780409838,37.03,-14.3959225765489));
#37686=CARTESIAN_POINT('',(10.192780409838,37.03,-14.3959225765489));
#37687=CARTESIAN_POINT('Origin',(10.1356594341564,37.03,-13.7749103120746));
#37688=CARTESIAN_POINT('',(10.1356594341564,37.03,-13.7749103120746));
#37689=CARTESIAN_POINT('Origin',(10.0358241714444,37.03,-13.1788877890042));
#37690=CARTESIAN_POINT('',(10.0358241714444,37.03,-13.1788877890042));
#37691=CARTESIAN_POINT('Origin',(9.89112836854343,37.03,-12.6120676561534));
#37692=CARTESIAN_POINT('',(9.89112836854343,37.03,-12.6120676561534));
#37693=CARTESIAN_POINT('Origin',(9.69653989065521,37.03,-12.0809901437375));
#37694=CARTESIAN_POINT('Origin',(9.23658232924928,37.03,-9.23658232924928));
#37695=CARTESIAN_POINT('',(9.23658232924928,37.03,-9.23658232924928));
#37696=CARTESIAN_POINT('Origin',(10.1351955192135,37.03,-8.24055326038936));
#37697=CARTESIAN_POINT('',(10.1351955192135,37.03,-8.24055326038936));
#37698=CARTESIAN_POINT('Origin',(11.6028715227817,37.03,-9.43386642869196));
#37699=CARTESIAN_POINT('',(11.6028715227817,37.03,-9.43386642869196));
#37700=CARTESIAN_POINT('Origin',(12.0809901437375,37.03,-9.69653989065521));
#37701=CARTESIAN_POINT('Origin',(13.7749103120746,37.03,-10.1356594341564));
#37702=CARTESIAN_POINT('',(13.7749103120746,37.03,-10.1356594341564));
#37703=CARTESIAN_POINT('Origin',(14.3959225765489,37.03,-10.192780409838));
#37704=CARTESIAN_POINT('',(14.3959225765489,37.03,-10.192780409838));
#37705=CARTESIAN_POINT('Origin',(15.0386712143394,37.03,-10.208136822609));
#37706=CARTESIAN_POINT('',(15.0386712143394,37.03,-10.208136822609));
#37707=CARTESIAN_POINT('Origin',(15.7003835976467,37.03,-10.1820769523934));
#37708=CARTESIAN_POINT('',(15.7003835976467,37.03,-10.1820769523934));
#37709=CARTESIAN_POINT('Origin',(16.3785524197668,37.03,-10.1146191541229));
#37710=CARTESIAN_POINT('',(16.3785524197668,37.03,-10.1146191541229));
#37711=CARTESIAN_POINT('Origin',(16.5265840124582,37.03,-9.87089260802485));
#37712=CARTESIAN_POINT('',(16.5265840124582,37.03,-9.87089260802485));
#37713=CARTESIAN_POINT('Origin',(16.6709890228504,37.03,-9.625));
#37714=CARTESIAN_POINT('',(16.6709890228504,37.03,-9.625));
#37715=CARTESIAN_POINT('Origin',(16.8117357628067,37.03,-9.37699528855417));
#37716=CARTESIAN_POINT('',(16.8117357628067,37.03,-9.37699528855417));
#37717=CARTESIAN_POINT('Origin',(16.9487933469585,37.03,-9.12693289567172));
#37718=CARTESIAN_POINT('',(16.9487933469585,37.03,-9.12693289567172));
#37719=CARTESIAN_POINT('Origin',(16.6681291028841,37.03,-8.50589256852586));
#37720=CARTESIAN_POINT('',(16.6681291028841,37.03,-8.50589256852586));
#37721=CARTESIAN_POINT('Origin',(16.3598414208564,37.03,-7.91980289947517));
#37722=CARTESIAN_POINT('',(16.3598414208564,37.03,-7.91980289947517));
#37723=CARTESIAN_POINT('Origin',(16.0251680583905,37.03,-7.37084445728621));
#37724=CARTESIAN_POINT('',(16.0251680583905,37.03,-7.37084445728621));
#37725=CARTESIAN_POINT('Origin',(15.6651937101241,37.03,-6.86159254803069));
#37726=CARTESIAN_POINT('',(15.6651937101241,37.03,-6.86159254803069));
#37727=CARTESIAN_POINT('Origin',(15.2807225748869,37.03,-6.39533953317997));
#37728=CARTESIAN_POINT('',(15.2807225748869,37.03,-6.39533953317997));
#37729=CARTESIAN_POINT('Origin',(14.8720022673282,37.03,-5.97680680020517));
#37730=CARTESIAN_POINT('',(14.8720022673282,37.03,-5.97680680020517));
#37731=CARTESIAN_POINT('Origin',(14.4379449459854,37.03,-5.6141744220185));
#37732=CARTESIAN_POINT('Origin',(12.617406105901,37.03,-3.38082377665168));
#37733=CARTESIAN_POINT('',(12.617406105901,37.03,-3.38082377665168));
#37734=CARTESIAN_POINT('Origin',(12.8976134221558,37.03,-2.0689307051291));
#37735=CARTESIAN_POINT('',(12.8976134221558,37.03,-2.0689307051291));
#37736=CARTESIAN_POINT('Origin',(14.765314709922,37.03,-2.36853222176556));
#37737=CARTESIAN_POINT('',(14.765314709922,37.03,-2.36853222176556));
#37738=CARTESIAN_POINT('Origin',(15.3107143126737,37.03,-2.35695480224783));
#37739=CARTESIAN_POINT('Origin',(16.997251982187,37.03,-1.8902833980495));
#37740=CARTESIAN_POINT('',(16.997251982187,37.03,-1.8902833980495));
#37741=CARTESIAN_POINT('Origin',(17.5636248671243,37.03,-1.62924548184168));
#37742=CARTESIAN_POINT('',(17.5636248671243,37.03,-1.62924548184168));
#37743=CARTESIAN_POINT('Origin',(18.1279397220842,37.03,-1.32117020651705));
#37744=CARTESIAN_POINT('',(18.1279397220842,37.03,-1.32117020651705));
#37745=CARTESIAN_POINT('Origin',(18.6879695209193,37.03,-0.967745505237384));
#37746=CARTESIAN_POINT('',(18.6879695209193,37.03,-0.967745505237384));
#37747=CARTESIAN_POINT('Origin',(19.2415520497946,37.03,-0.570240927191682));
#37748=CARTESIAN_POINT('',(19.2415520497946,37.03,-0.570240927191682));
#37749=CARTESIAN_POINT('Origin',(19.247887896579,37.03,-0.285151750348434));
#37750=CARTESIAN_POINT('',(19.247887896579,37.03,-0.285151750348434));
#37751=CARTESIAN_POINT('Origin',(19.25,37.03,0.));
#37752=CARTESIAN_POINT('',(19.25,37.03,0.));
#37753=CARTESIAN_POINT('Origin',(19.247887896579,37.03,0.285151750348434));
#37754=CARTESIAN_POINT('',(19.247887896579,37.03,0.285151750348434));
#37755=CARTESIAN_POINT('Origin',(19.2415520497946,37.03,0.570240927191682));
#37756=CARTESIAN_POINT('',(19.2415520497946,37.03,0.570240927191682));
#37757=CARTESIAN_POINT('Origin',(18.6879695209193,37.03,0.967745505237384));
#37758=CARTESIAN_POINT('',(18.6879695209193,37.03,0.967745505237384));
#37759=CARTESIAN_POINT('Origin',(18.1279397220842,37.03,1.32117020651705));
#37760=CARTESIAN_POINT('',(18.1279397220842,37.03,1.32117020651705));
#37761=CARTESIAN_POINT('Origin',(17.5636248671243,37.03,1.62924548184168));
#37762=CARTESIAN_POINT('',(17.5636248671243,37.03,1.62924548184168));
#37763=CARTESIAN_POINT('Origin',(16.997251982187,37.03,1.8902833980495));
#37764=CARTESIAN_POINT('',(16.997251982187,37.03,1.8902833980495));
#37765=CARTESIAN_POINT('Origin',(16.4311637046244,37.03,2.10183478588267));
#37766=CARTESIAN_POINT('',(16.4311637046244,37.03,2.10183478588267));
#37767=CARTESIAN_POINT('Origin',(15.8679351687486,37.03,2.25993461117485));
#37768=CARTESIAN_POINT('',(15.8679351687486,37.03,2.25993461117485));
#37769=CARTESIAN_POINT('Origin',(15.3107143126737,37.03,2.35695480224783));
#37770=CARTESIAN_POINT('Origin',(12.617406105901,37.03,3.38082377665168));
#37771=CARTESIAN_POINT('',(12.617406105901,37.03,3.38082377665168));
#37772=CARTESIAN_POINT('Origin',(12.2041262243426,37.03,4.65706016176646));
#37773=CARTESIAN_POINT('',(12.2041262243426,37.03,4.65706016176646));
#37774=CARTESIAN_POINT('Origin',(13.9714037445473,37.03,5.33144828123002));
#37775=CARTESIAN_POINT('',(13.9714037445473,37.03,5.33144828123002));
#37776=CARTESIAN_POINT('Origin',(14.4379449459854,37.03,5.6141744220185));
#37777=CARTESIAN_POINT('Origin',(15.6651937101241,37.03,6.86159254803069));
#37778=CARTESIAN_POINT('',(15.6651937101241,37.03,6.86159254803069));
#37779=CARTESIAN_POINT('Origin',(16.0251680583905,37.03,7.37084445728621));
#37780=CARTESIAN_POINT('',(16.0251680583905,37.03,7.37084445728621));
#37781=CARTESIAN_POINT('Origin',(16.3598414208564,37.03,7.91980289947517));
#37782=CARTESIAN_POINT('',(16.3598414208564,37.03,7.91980289947517));
#37783=CARTESIAN_POINT('Origin',(16.6681291028841,37.03,8.50589256852586));
#37784=CARTESIAN_POINT('',(16.6681291028841,37.03,8.50589256852586));
#37785=CARTESIAN_POINT('Origin',(16.9487933469585,37.03,9.12693289567172));
#37786=CARTESIAN_POINT('',(16.9487933469585,37.03,9.12693289567172));
#37787=CARTESIAN_POINT('Origin',(16.8117357628067,37.03,9.37699528855417));
#37788=CARTESIAN_POINT('',(16.8117357628067,37.03,9.37699528855417));
#37789=CARTESIAN_POINT('Origin',(16.6709890228504,37.03,9.625));
#37790=CARTESIAN_POINT('',(16.6709890228504,37.03,9.625));
#37791=CARTESIAN_POINT('Origin',(16.5265840124582,37.03,9.87089260802485));
#37792=CARTESIAN_POINT('',(16.5265840124582,37.03,9.87089260802485));
#37793=CARTESIAN_POINT('Origin',(16.3785524197668,37.03,10.1146191541229));
#37794=CARTESIAN_POINT('',(16.3785524197668,37.03,10.1146191541229));
#37795=CARTESIAN_POINT('Origin',(15.7003835976467,37.03,10.1820769523934));
#37796=CARTESIAN_POINT('',(15.7003835976467,37.03,10.1820769523934));
#37797=CARTESIAN_POINT('Origin',(15.0386712143394,37.03,10.208136822609));
#37798=CARTESIAN_POINT('',(15.0386712143394,37.03,10.208136822609));
#37799=CARTESIAN_POINT('Origin',(14.3959225765489,37.03,10.192780409838));
#37800=CARTESIAN_POINT('',(14.3959225765489,37.03,10.192780409838));
#37801=CARTESIAN_POINT('Origin',(13.7749103120746,37.03,10.1356594341564));
#37802=CARTESIAN_POINT('',(13.7749103120746,37.03,10.1356594341564));
#37803=CARTESIAN_POINT('Origin',(13.1788877890042,37.03,10.0358241714444));
#37804=CARTESIAN_POINT('',(13.1788877890042,37.03,10.0358241714444));
#37805=CARTESIAN_POINT('Origin',(12.6120676561534,37.03,9.89112836854343));
#37806=CARTESIAN_POINT('',(12.6120676561534,37.03,9.89112836854343));
#37807=CARTESIAN_POINT('Origin',(12.0809901437375,37.03,9.69653989065521));
#37808=CARTESIAN_POINT('Origin',(9.23658232924928,37.03,9.23658232924928));
#37809=CARTESIAN_POINT('',(9.23658232924928,37.03,9.23658232924928));
#37810=CARTESIAN_POINT('Origin',(8.24055326038937,37.03,10.1351955192135));
#37811=CARTESIAN_POINT('',(8.24055326038937,37.03,10.1351955192135));
#37812=CARTESIAN_POINT('Origin',(9.43386642869196,37.03,11.6028715227817));
#37813=CARTESIAN_POINT('',(9.43386642869196,37.03,11.6028715227817));
#37814=CARTESIAN_POINT('Origin',(9.69653989065521,37.03,12.0809901437375));
#37815=CARTESIAN_POINT('Origin',(10.1356594341564,37.03,13.7749103120746));
#37816=CARTESIAN_POINT('',(10.1356594341564,37.03,13.7749103120746));
#37817=CARTESIAN_POINT('Origin',(10.192780409838,37.03,14.3959225765489));
#37818=CARTESIAN_POINT('',(10.192780409838,37.03,14.3959225765489));
#37819=CARTESIAN_POINT('Origin',(10.208136822609,37.03,15.0386712143394));
#37820=CARTESIAN_POINT('',(10.208136822609,37.03,15.0386712143394));
#37821=CARTESIAN_POINT('Origin',(10.1820769523934,37.03,15.7003835976467));
#37822=CARTESIAN_POINT('',(10.1820769523934,37.03,15.7003835976467));
#37823=CARTESIAN_POINT('Origin',(10.1146191541229,37.03,16.3785524197668));
#37824=CARTESIAN_POINT('',(10.1146191541229,37.03,16.3785524197668));
#37825=CARTESIAN_POINT('Origin',(9.87089260802485,37.03,16.5265840124582));
#37826=CARTESIAN_POINT('',(9.87089260802485,37.03,16.5265840124582));
#37827=CARTESIAN_POINT('Origin',(9.625,37.03,16.6709890228504));
#37828=CARTESIAN_POINT('',(9.625,37.03,16.6709890228504));
#37829=CARTESIAN_POINT('Origin',(9.37699528855417,37.03,16.8117357628067));
#37830=CARTESIAN_POINT('',(9.37699528855417,37.03,16.8117357628067));
#37831=CARTESIAN_POINT('Origin',(9.12693289567173,37.03,16.9487933469585));
#37832=CARTESIAN_POINT('',(9.12693289567173,37.03,16.9487933469585));
#37833=CARTESIAN_POINT('Origin',(8.50589256852587,37.03,16.6681291028841));
#37834=CARTESIAN_POINT('',(8.50589256852587,37.03,16.6681291028841));
#37835=CARTESIAN_POINT('Origin',(7.91980289947518,37.03,16.3598414208564));
#37836=CARTESIAN_POINT('',(7.91980289947518,37.03,16.3598414208564));
#37837=CARTESIAN_POINT('Origin',(7.37084445728622,37.03,16.0251680583905));
#37838=CARTESIAN_POINT('',(7.37084445728622,37.03,16.0251680583905));
#37839=CARTESIAN_POINT('Origin',(6.86159254803069,37.03,15.6651937101241));
#37840=CARTESIAN_POINT('',(6.86159254803069,37.03,15.6651937101241));
#37841=CARTESIAN_POINT('Origin',(6.39533953317997,37.03,15.2807225748869));
#37842=CARTESIAN_POINT('',(6.39533953317997,37.03,15.2807225748869));
#37843=CARTESIAN_POINT('Origin',(5.97680680020517,37.03,14.8720022673282));
#37844=CARTESIAN_POINT('',(5.97680680020517,37.03,14.8720022673282));
#37845=CARTESIAN_POINT('Origin',(5.61417442201851,37.03,14.4379449459854));
#37846=CARTESIAN_POINT('Origin',(3.38082377665168,37.03,12.617406105901));
#37847=CARTESIAN_POINT('',(3.38082377665168,37.03,12.617406105901));
#37848=CARTESIAN_POINT('Origin',(2.0689307051291,37.03,12.8976134221558));
#37849=CARTESIAN_POINT('',(2.0689307051291,37.03,12.8976134221558));
#37850=CARTESIAN_POINT('Origin',(2.36853222176556,37.03,14.765314709922));
#37851=CARTESIAN_POINT('',(2.36853222176556,37.03,14.765314709922));
#37852=CARTESIAN_POINT('Origin',(2.35695480224784,37.03,15.3107143126737));
#37853=CARTESIAN_POINT('Origin',(1.8902833980495,37.03,16.997251982187));
#37854=CARTESIAN_POINT('',(1.8902833980495,37.03,16.997251982187));
#37855=CARTESIAN_POINT('Origin',(1.62924548184168,37.03,17.5636248671243));
#37856=CARTESIAN_POINT('',(1.62924548184168,37.03,17.5636248671243));
#37857=CARTESIAN_POINT('Origin',(1.32117020651705,37.03,18.1279397220842));
#37858=CARTESIAN_POINT('',(1.32117020651705,37.03,18.1279397220842));
#37859=CARTESIAN_POINT('Origin',(0.967745505237385,37.03,18.6879695209193));
#37860=CARTESIAN_POINT('',(0.967745505237385,37.03,18.6879695209193));
#37861=CARTESIAN_POINT('Origin',(0.570240927191682,37.03,19.2415520497946));
#37862=CARTESIAN_POINT('',(0.570240927191682,37.03,19.2415520497946));
#37863=CARTESIAN_POINT('Origin',(0.285151750348434,37.03,19.247887896579));
#37864=CARTESIAN_POINT('',(0.285151750348434,37.03,19.247887896579));
#37865=CARTESIAN_POINT('Origin',(1.17961196366423E-15,37.03,19.25));
#37866=CARTESIAN_POINT('',(1.17872254417933E-15,37.03,19.25));
#37867=CARTESIAN_POINT('Origin',(-0.285151750348432,37.03,19.247887896579));
#37868=CARTESIAN_POINT('',(-0.285151750348432,37.03,19.247887896579));
#37869=CARTESIAN_POINT('Origin',(-0.57024092719168,37.03,19.2415520497946));
#37870=CARTESIAN_POINT('',(-0.57024092719168,37.03,19.2415520497946));
#37871=CARTESIAN_POINT('Origin',(-0.967745505237382,37.03,18.6879695209193));
#37872=CARTESIAN_POINT('',(-0.967745505237382,37.03,18.6879695209193));
#37873=CARTESIAN_POINT('Origin',(-1.32117020651705,37.03,18.1279397220842));
#37874=CARTESIAN_POINT('',(-1.32117020651705,37.03,18.1279397220842));
#37875=CARTESIAN_POINT('Origin',(-1.62924548184168,37.03,17.5636248671243));
#37876=CARTESIAN_POINT('',(-1.62924548184168,37.03,17.5636248671243));
#37877=CARTESIAN_POINT('Origin',(-1.8902833980495,37.03,16.997251982187));
#37878=CARTESIAN_POINT('',(-1.8902833980495,37.03,16.997251982187));
#37879=CARTESIAN_POINT('Origin',(-2.10183478588267,37.03,16.4311637046244));
#37880=CARTESIAN_POINT('',(-2.10183478588267,37.03,16.4311637046244));
#37881=CARTESIAN_POINT('Origin',(-2.25993461117485,37.03,15.8679351687486));
#37882=CARTESIAN_POINT('',(-2.25993461117485,37.03,15.8679351687486));
#37883=CARTESIAN_POINT('Origin',(-2.35695480224783,37.03,15.3107143126737));
#37884=CARTESIAN_POINT('Origin',(-3.38082377665168,37.03,12.617406105901));
#37885=CARTESIAN_POINT('',(-3.38082377665168,37.03,12.617406105901));
#37886=CARTESIAN_POINT('Origin',(-4.65706016176645,37.03,12.2041262243426));
#37887=CARTESIAN_POINT('',(-4.65706016176645,37.03,12.2041262243426));
#37888=CARTESIAN_POINT('Origin',(-5.33144828123002,37.03,13.9714037445473));
#37889=CARTESIAN_POINT('',(-5.33144828123002,37.03,13.9714037445473));
#37890=CARTESIAN_POINT('Origin',(-5.6141744220185,37.03,14.4379449459854));
#37891=CARTESIAN_POINT('Origin',(-6.86159254803068,37.03,15.6651937101241));
#37892=CARTESIAN_POINT('',(-6.86159254803068,37.03,15.6651937101241));
#37893=CARTESIAN_POINT('Origin',(-7.37084445728621,37.03,16.0251680583905));
#37894=CARTESIAN_POINT('',(-7.37084445728621,37.03,16.0251680583905));
#37895=CARTESIAN_POINT('Origin',(-7.91980289947517,37.03,16.3598414208564));
#37896=CARTESIAN_POINT('',(-7.91980289947517,37.03,16.3598414208564));
#37897=CARTESIAN_POINT('Origin',(-8.50589256852586,37.03,16.6681291028841));
#37898=CARTESIAN_POINT('',(-8.50589256852586,37.03,16.6681291028841));
#37899=CARTESIAN_POINT('Origin',(-9.12693289567172,37.03,16.9487933469585));
#37900=CARTESIAN_POINT('',(-9.12693289567172,37.03,16.9487933469585));
#37901=CARTESIAN_POINT('Origin',(-9.37699528855417,37.03,16.8117357628067));
#37902=CARTESIAN_POINT('',(-9.37699528855417,37.03,16.8117357628067));
#37903=CARTESIAN_POINT('Origin',(-9.625,37.03,16.6709890228504));
#37904=CARTESIAN_POINT('',(-9.625,37.03,16.6709890228504));
#37905=CARTESIAN_POINT('Origin',(-9.87089260802485,37.03,16.5265840124582));
#37906=CARTESIAN_POINT('',(-9.87089260802485,37.03,16.5265840124582));
#37907=CARTESIAN_POINT('Origin',(-10.1146191541229,37.03,16.3785524197668));
#37908=CARTESIAN_POINT('',(-10.1146191541229,37.03,16.3785524197668));
#37909=CARTESIAN_POINT('Origin',(-10.1820769523934,37.03,15.7003835976467));
#37910=CARTESIAN_POINT('',(-10.1820769523934,37.03,15.7003835976467));
#37911=CARTESIAN_POINT('Origin',(-10.208136822609,37.03,15.0386712143394));
#37912=CARTESIAN_POINT('',(-10.208136822609,37.03,15.0386712143394));
#37913=CARTESIAN_POINT('Origin',(-10.192780409838,37.03,14.3959225765489));
#37914=CARTESIAN_POINT('',(-10.192780409838,37.03,14.3959225765489));
#37915=CARTESIAN_POINT('Origin',(-10.1356594341564,37.03,13.7749103120746));
#37916=CARTESIAN_POINT('',(-10.1356594341564,37.03,13.7749103120746));
#37917=CARTESIAN_POINT('Origin',(-10.0358241714444,37.03,13.1788877890042));
#37918=CARTESIAN_POINT('',(-10.0358241714444,37.03,13.1788877890042));
#37919=CARTESIAN_POINT('Origin',(-9.89112836854343,37.03,12.6120676561534));
#37920=CARTESIAN_POINT('',(-9.89112836854343,37.03,12.6120676561534));
#37921=CARTESIAN_POINT('Origin',(-9.6965398906552,37.03,12.0809901437375));
#37922=CARTESIAN_POINT('Origin',(-9.23658232924928,37.03,9.23658232924928));
#37923=CARTESIAN_POINT('',(-9.23658232924928,37.03,9.23658232924928));
#37924=CARTESIAN_POINT('Origin',(-10.1351955192135,37.03,8.24055326038937));
#37925=CARTESIAN_POINT('',(-10.1351955192135,37.03,8.24055326038937));
#37926=CARTESIAN_POINT('Origin',(-11.6028715227817,37.03,9.43386642869196));
#37927=CARTESIAN_POINT('',(-11.6028715227817,37.03,9.43386642869196));
#37928=CARTESIAN_POINT('Origin',(-12.0809901437375,37.03,9.69653989065521));
#37929=CARTESIAN_POINT('Origin',(-13.7749103120746,37.03,10.1356594341564));
#37930=CARTESIAN_POINT('',(-13.7749103120746,37.03,10.1356594341564));
#37931=CARTESIAN_POINT('Origin',(-14.3959225765489,37.03,10.192780409838));
#37932=CARTESIAN_POINT('',(-14.3959225765489,37.03,10.192780409838));
#37933=CARTESIAN_POINT('Origin',(-15.0386712143394,37.03,10.208136822609));
#37934=CARTESIAN_POINT('',(-15.0386712143394,37.03,10.208136822609));
#37935=CARTESIAN_POINT('Origin',(-15.7003835976467,37.03,10.1820769523934));
#37936=CARTESIAN_POINT('',(-15.7003835976467,37.03,10.1820769523934));
#37937=CARTESIAN_POINT('Origin',(-16.3785524197668,37.03,10.1146191541229));
#37938=CARTESIAN_POINT('',(-16.3785524197668,37.03,10.1146191541229));
#37939=CARTESIAN_POINT('Origin',(-16.5265840124582,37.03,9.87089260802485));
#37940=CARTESIAN_POINT('',(-16.5265840124582,37.03,9.87089260802485));
#37941=CARTESIAN_POINT('Origin',(-16.6709890228504,37.03,9.625));
#37942=CARTESIAN_POINT('',(-16.6709890228504,37.03,9.625));
#37943=CARTESIAN_POINT('Origin',(-16.8117357628067,37.03,9.37699528855417));
#37944=CARTESIAN_POINT('',(-16.8117357628067,37.03,9.37699528855417));
#37945=CARTESIAN_POINT('Origin',(-16.9487933469585,37.03,9.12693289567172));
#37946=CARTESIAN_POINT('',(-16.9487933469585,37.03,9.12693289567172));
#37947=CARTESIAN_POINT('Origin',(-16.6681291028841,37.03,8.50589256852586));
#37948=CARTESIAN_POINT('',(-16.6681291028841,37.03,8.50589256852586));
#37949=CARTESIAN_POINT('Origin',(-16.3598414208564,37.03,7.91980289947518));
#37950=CARTESIAN_POINT('',(-16.3598414208564,37.03,7.91980289947518));
#37951=CARTESIAN_POINT('Origin',(-16.0251680583905,37.03,7.37084445728621));
#37952=CARTESIAN_POINT('',(-16.0251680583905,37.03,7.37084445728621));
#37953=CARTESIAN_POINT('Origin',(-15.6651937101241,37.03,6.86159254803069));
#37954=CARTESIAN_POINT('',(-15.6651937101241,37.03,6.86159254803069));
#37955=CARTESIAN_POINT('Origin',(-15.2807225748869,37.03,6.39533953317997));
#37956=CARTESIAN_POINT('',(-15.2807225748869,37.03,6.39533953317997));
#37957=CARTESIAN_POINT('Origin',(-14.8720022673282,37.03,5.97680680020517));
#37958=CARTESIAN_POINT('',(-14.8720022673282,37.03,5.97680680020517));
#37959=CARTESIAN_POINT('Origin',(-14.4379449459854,37.03,5.61417442201851));
#37960=CARTESIAN_POINT('Origin',(-12.617406105901,37.03,3.38082377665168));
#37961=CARTESIAN_POINT('',(-12.617406105901,37.03,3.38082377665168));
#37962=CARTESIAN_POINT('Origin',(-12.8976134221558,37.03,2.0689307051291));
#37963=CARTESIAN_POINT('',(-12.8976134221558,37.03,2.0689307051291));
#37964=CARTESIAN_POINT('Origin',(-14.765314709922,37.03,2.36853222176556));
#37965=CARTESIAN_POINT('',(-14.765314709922,37.03,2.36853222176556));
#37966=CARTESIAN_POINT('Origin',(-15.3107143126737,37.03,2.35695480224783));
#37967=CARTESIAN_POINT('Origin',(-16.997251982187,37.03,1.8902833980495));
#37968=CARTESIAN_POINT('',(-16.997251982187,37.03,1.8902833980495));
#37969=CARTESIAN_POINT('Origin',(-17.5636248671243,37.03,1.62924548184169));
#37970=CARTESIAN_POINT('',(-17.5636248671243,37.03,1.62924548184169));
#37971=CARTESIAN_POINT('Origin',(-18.1279397220842,37.03,1.32117020651705));
#37972=CARTESIAN_POINT('',(-18.1279397220842,37.03,1.32117020651705));
#37973=CARTESIAN_POINT('Origin',(-18.6879695209193,37.03,0.96774550523739));
#37974=CARTESIAN_POINT('',(-18.6879695209193,37.03,0.96774550523739));
#37975=CARTESIAN_POINT('Origin',(-19.2415520497946,37.03,0.570240927191683));
#37976=CARTESIAN_POINT('',(-19.2415520497946,37.03,0.570240927191683));
#37977=CARTESIAN_POINT('Origin',(-19.247887896579,37.03,0.285151750348435));
#37978=CARTESIAN_POINT('',(-19.247887896579,37.03,0.285151750348435));
#37979=CARTESIAN_POINT('Origin',(-19.25,37.03,2.35922392732846E-15));
#37980=CARTESIAN_POINT('',(-19.25,37.03,2.35744508835865E-15));
#37981=CARTESIAN_POINT('Origin',(-19.247887896579,37.03,-0.285151750348431));
#37982=CARTESIAN_POINT('',(-19.247887896579,37.03,-0.285151750348431));
#37983=CARTESIAN_POINT('Origin',(-19.2415520497946,37.03,-0.570240927191679));
#37984=CARTESIAN_POINT('',(-19.2415520497946,37.03,-0.570240927191679));
#37985=CARTESIAN_POINT('Origin',(-18.6879695209193,37.03,-0.967745505237385));
#37986=CARTESIAN_POINT('',(-18.6879695209193,37.03,-0.967745505237385));
#37987=CARTESIAN_POINT('Origin',(-18.1279397220842,37.03,-1.32117020651705));
#37988=CARTESIAN_POINT('',(-18.1279397220842,37.03,-1.32117020651705));
#37989=CARTESIAN_POINT('Origin',(-17.5636248671243,37.03,-1.62924548184168));
#37990=CARTESIAN_POINT('',(-17.5636248671243,37.03,-1.62924548184168));
#37991=CARTESIAN_POINT('Origin',(-16.997251982187,37.03,-1.89028339804949));
#37992=CARTESIAN_POINT('',(-16.997251982187,37.03,-1.89028339804949));
#37993=CARTESIAN_POINT('Origin',(-16.4311637046244,37.03,-2.10183478588267));
#37994=CARTESIAN_POINT('',(-16.4311637046244,37.03,-2.10183478588267));
#37995=CARTESIAN_POINT('Origin',(-15.8679351687486,37.03,-2.25993461117485));
#37996=CARTESIAN_POINT('',(-15.8679351687486,37.03,-2.25993461117485));
#37997=CARTESIAN_POINT('Origin',(-15.3107143126737,37.03,-2.35695480224783));
#37998=CARTESIAN_POINT('Origin',(-12.617406105901,37.03,-3.38082377665168));
#37999=CARTESIAN_POINT('',(-12.617406105901,37.03,-3.38082377665168));
#38000=CARTESIAN_POINT('Origin',(-12.2041262243426,37.03,-4.65706016176646));
#38001=CARTESIAN_POINT('',(-12.2041262243426,37.03,-4.65706016176646));
#38002=CARTESIAN_POINT('Origin',(-13.9714037445473,37.03,-5.33144828123002));
#38003=CARTESIAN_POINT('',(-13.9714037445473,37.03,-5.33144828123002));
#38004=CARTESIAN_POINT('Origin',(-14.4379449459854,37.03,-5.61417442201851));
#38005=CARTESIAN_POINT('Origin',(-15.6651937101241,37.03,-6.86159254803069));
#38006=CARTESIAN_POINT('',(-15.6651937101241,37.03,-6.86159254803069));
#38007=CARTESIAN_POINT('Origin',(-16.0251680583905,37.03,-7.37084445728622));
#38008=CARTESIAN_POINT('',(-16.0251680583905,37.03,-7.37084445728622));
#38009=CARTESIAN_POINT('Origin',(-16.3598414208564,37.03,-7.91980289947518));
#38010=CARTESIAN_POINT('',(-16.3598414208564,37.03,-7.91980289947518));
#38011=CARTESIAN_POINT('Origin',(-16.6681291028841,37.03,-8.50589256852587));
#38012=CARTESIAN_POINT('',(-16.6681291028841,37.03,-8.50589256852587));
#38013=CARTESIAN_POINT('Origin',(-16.9487933469585,37.03,-9.12693289567173));
#38014=CARTESIAN_POINT('',(-16.9487933469585,37.03,-9.12693289567173));
#38015=CARTESIAN_POINT('Origin',(-16.8117357628067,37.03,-9.37699528855417));
#38016=CARTESIAN_POINT('',(-16.8117357628067,37.03,-9.37699528855417));
#38017=CARTESIAN_POINT('Origin',(-16.6709890228504,37.03,-9.625));
#38018=CARTESIAN_POINT('',(-16.6709890228504,37.03,-9.625));
#38019=CARTESIAN_POINT('Origin',(-16.5265840124582,37.03,-9.87089260802485));
#38020=CARTESIAN_POINT('',(-16.5265840124582,37.03,-9.87089260802485));
#38021=CARTESIAN_POINT('Origin',(-16.3785524197668,37.03,-10.1146191541229));
#38022=CARTESIAN_POINT('',(-16.3785524197668,37.03,-10.1146191541229));
#38023=CARTESIAN_POINT('Origin',(-15.7003835976467,37.03,-10.1820769523934));
#38024=CARTESIAN_POINT('',(-15.7003835976467,37.03,-10.1820769523934));
#38025=CARTESIAN_POINT('Origin',(-15.0386712143394,37.03,-10.208136822609));
#38026=CARTESIAN_POINT('',(-15.0386712143394,37.03,-10.208136822609));
#38027=CARTESIAN_POINT('Origin',(-14.3959225765489,37.03,-10.192780409838));
#38028=CARTESIAN_POINT('',(-14.3959225765489,37.03,-10.192780409838));
#38029=CARTESIAN_POINT('Origin',(-13.7749103120746,37.03,-10.1356594341564));
#38030=CARTESIAN_POINT('',(-13.7749103120746,37.03,-10.1356594341564));
#38031=CARTESIAN_POINT('Origin',(-13.1788877890042,37.03,-10.0358241714444));
#38032=CARTESIAN_POINT('',(-13.1788877890042,37.03,-10.0358241714444));
#38033=CARTESIAN_POINT('Origin',(-12.6120676561534,37.03,-9.89112836854343));
#38034=CARTESIAN_POINT('',(-12.6120676561534,37.03,-9.89112836854343));
#38035=CARTESIAN_POINT('Origin',(-12.0809901437375,37.03,-9.69653989065521));
#38036=CARTESIAN_POINT('Origin',(-9.23658232924928,37.03,-9.23658232924928));
#38037=CARTESIAN_POINT('',(-9.23658232924928,37.03,-9.23658232924928));
#38038=CARTESIAN_POINT('Origin',(-8.24055326038937,37.03,-10.1351955192135));
#38039=CARTESIAN_POINT('',(-8.24055326038937,37.03,-10.1351955192135));
#38040=CARTESIAN_POINT('Origin',(-9.43386642869197,37.03,-11.6028715227817));
#38041=CARTESIAN_POINT('',(-9.43386642869197,37.03,-11.6028715227817));
#38042=CARTESIAN_POINT('Origin',(-9.69653989065522,37.03,-12.0809901437375));
#38043=CARTESIAN_POINT('Origin',(-10.1356594341564,37.03,-13.7749103120746));
#38044=CARTESIAN_POINT('',(-10.1356594341564,37.03,-13.7749103120746));
#38045=CARTESIAN_POINT('Origin',(-10.192780409838,37.03,-14.3959225765489));
#38046=CARTESIAN_POINT('',(-10.192780409838,37.03,-14.3959225765489));
#38047=CARTESIAN_POINT('Origin',(-10.208136822609,37.03,-15.0386712143394));
#38048=CARTESIAN_POINT('',(-10.208136822609,37.03,-15.0386712143394));
#38049=CARTESIAN_POINT('Origin',(-10.1820769523934,37.03,-15.7003835976467));
#38050=CARTESIAN_POINT('',(-10.1820769523934,37.03,-15.7003835976467));
#38051=CARTESIAN_POINT('Origin',(-10.1146191541229,37.03,-16.3785524197668));
#38052=CARTESIAN_POINT('',(-10.1146191541229,37.03,-16.3785524197668));
#38053=CARTESIAN_POINT('Origin',(-9.87089260802487,37.03,-16.5265840124582));
#38054=CARTESIAN_POINT('',(-9.87089260802487,37.03,-16.5265840124582));
#38055=CARTESIAN_POINT('Origin',(-9.62500000000001,37.03,-16.6709890228504));
#38056=CARTESIAN_POINT('',(-9.62500000000001,37.03,-16.6709890228504));
#38057=CARTESIAN_POINT('Origin',(-9.37699528855417,37.03,-16.8117357628067));
#38058=CARTESIAN_POINT('',(-9.37699528855417,37.03,-16.8117357628067));
#38059=CARTESIAN_POINT('Origin',(-9.12693289567173,37.03,-16.9487933469585));
#38060=CARTESIAN_POINT('',(-9.12693289567173,37.03,-16.9487933469585));
#38061=CARTESIAN_POINT('Origin',(-8.50589256852587,37.03,-16.6681291028841));
#38062=CARTESIAN_POINT('',(-8.50589256852587,37.03,-16.6681291028841));
#38063=CARTESIAN_POINT('Origin',(-7.91980289947518,37.03,-16.3598414208564));
#38064=CARTESIAN_POINT('',(-7.91980289947518,37.03,-16.3598414208564));
#38065=CARTESIAN_POINT('Origin',(-7.37084445728623,37.03,-16.0251680583905));
#38066=CARTESIAN_POINT('',(-7.37084445728623,37.03,-16.0251680583905));
#38067=CARTESIAN_POINT('Origin',(-6.86159254803069,37.03,-15.6651937101241));
#38068=CARTESIAN_POINT('',(-6.86159254803069,37.03,-15.6651937101241));
#38069=CARTESIAN_POINT('Origin',(-6.39533953317998,37.03,-15.2807225748869));
#38070=CARTESIAN_POINT('',(-6.39533953317998,37.03,-15.2807225748869));
#38071=CARTESIAN_POINT('Origin',(-5.97680680020517,37.03,-14.8720022673282));
#38072=CARTESIAN_POINT('',(-5.97680680020517,37.03,-14.8720022673282));
#38073=CARTESIAN_POINT('Origin',(-5.61417442201851,37.03,-14.4379449459854));
#38074=CARTESIAN_POINT('Origin',(-3.38082377665168,37.03,-12.617406105901));
#38075=CARTESIAN_POINT('Origin',(0.,51.,0.));
#38076=CARTESIAN_POINT('',(-1.04094977927525E-15,18.05,-8.5));
#38077=CARTESIAN_POINT('',(-1.04094977927525E-15,51.,-8.5));
#38078=CARTESIAN_POINT('Origin',(0.,18.05,0.));
#38079=CARTESIAN_POINT('Origin',(0.,-37.8,7.44));
#38080=CARTESIAN_POINT('',(-9.11137218565631E-16,-37.8,-7.44));
#38081=CARTESIAN_POINT('Origin',(0.,-37.8,0.));
#38082=CARTESIAN_POINT('Origin',(0.,-37.55,0.));
#38083=CARTESIAN_POINT('',(-9.72369558522998E-16,-37.3,-7.93999999999999));
#38084=CARTESIAN_POINT('Origin',(0.,-37.3,0.));
#38085=CARTESIAN_POINT('',(-9.41753388544315E-16,-37.55,-7.69));
#38086=CARTESIAN_POINT('Origin',(0.,-9.62499999999999,0.));
#38087=CARTESIAN_POINT('',(-9.72369558522999E-16,18.05,-7.94));
#38088=CARTESIAN_POINT('Origin',(0.,18.05,0.));
#38089=CARTESIAN_POINT('',(-9.72369558522999E-16,-9.62499999999999,-7.94));
#38090=CARTESIAN_POINT('Origin',(0.,18.05,8.5));
#38091=CARTESIAN_POINT('Origin',(0.,51.,0.));
#38092=CARTESIAN_POINT('',(-1.04094977927525E-15,83.95,-8.5));
#38093=CARTESIAN_POINT('Origin',(0.,83.95,0.));
#38094=CARTESIAN_POINT('',(-1.04094977927525E-15,51.,-8.5));
#38095=CARTESIAN_POINT('Origin',(0.,83.95,0.));
#38096=CARTESIAN_POINT('',(0.,0.,0.));
#38097=CARTESIAN_POINT('Origin',(5.91118355257506,37.28,-28.4145311199496));
#38098=CARTESIAN_POINT('',(12.8183396498506,37.2481324154382,-23.3776905273493));
#38099=CARTESIAN_POINT('',(13.0730690072096,37.03,-22.9241469865312));
#38100=CARTESIAN_POINT('',(11.3376395086249,38.5161005118286,-26.014065038336));
#38101=CARTESIAN_POINT('',(10.3106808445568,37.03,-24.9228064432661));
#38102=CARTESIAN_POINT('',(5.76463742854583,37.03,-28.2119867210341));
#38103=CARTESIAN_POINT('',(10.5829448433309,37.53,-25.3429650194728));
#38104=CARTESIAN_POINT('',(10.4860359897738,37.3520314584495,-25.1934150014179));
#38105=CARTESIAN_POINT('',(12.1154593532086,37.53,-24.23415103773));
#38106=CARTESIAN_POINT('',(6.05772967660429,37.53,-28.617075518865));
#38107=CARTESIAN_POINT('',(12.4929286389212,37.4321844925501,-23.8403088083181));
#38108=CARTESIAN_POINT('',(9.89277877754194,38.1059743550985,-26.5532416401305));
#38109=CARTESIAN_POINT('',(10.7287682421066,38.4299914950389,-26.3483150610773));
#38110=CARTESIAN_POINT('Origin',(2.22044604925031E-15,37.03,-33.));
#38111=CARTESIAN_POINT('',(11.3124568369342,37.03,-26.46875));
#38112=CARTESIAN_POINT('',(11.3124568369342,37.03,-26.46875));
#38113=CARTESIAN_POINT('',(13.1048089083576,37.03,-22.8676343517052));
#38114=CARTESIAN_POINT('',(12.8183396498506,37.03,-23.3776905273493));
#38115=CARTESIAN_POINT('',(13.3555043472661,37.03,-22.3177600709842));
#38116=CARTESIAN_POINT('',(13.1048089083576,37.03,-22.8676343517052));
#38117=CARTESIAN_POINT('',(13.571408774188,37.03,-21.7326922826676));
#38118=CARTESIAN_POINT('',(13.3555043472661,37.03,-22.3177600709842));
#38119=CARTESIAN_POINT('',(13.7525975185565,37.03,-21.1158193057032));
#38120=CARTESIAN_POINT('',(13.571408774188,37.03,-21.7326922826676));
#38121=CARTESIAN_POINT('',(13.8986893840657,37.03,-20.4699094343666));
#38122=CARTESIAN_POINT('',(13.7525975185565,37.03,-21.1158193057032));
#38123=CARTESIAN_POINT('',(14.009053161491,37.03,-19.7973892915637));
#38124=CARTESIAN_POINT('',(13.8986893840657,37.03,-20.4699094343666));
#38125=CARTESIAN_POINT('',(13.8119447915281,37.03,-19.5913206811491));
#38126=CARTESIAN_POINT('',(14.009053161491,37.03,-19.7973892915637));
#38127=CARTESIAN_POINT('',(13.611805537841,37.03,-19.388194462159));
#38128=CARTESIAN_POINT('',(13.8119447915281,37.03,-19.5913206811491));
#38129=CARTESIAN_POINT('',(13.4086793188509,37.03,-19.1880552084719));
#38130=CARTESIAN_POINT('',(13.611805537841,37.03,-19.388194462159));
#38131=CARTESIAN_POINT('',(13.2026107084364,37.03,-18.990946838509));
#38132=CARTESIAN_POINT('',(13.4086793188509,37.03,-19.1880552084719));
#38133=CARTESIAN_POINT('',(12.5300905656334,37.03,-19.1013106159343));
#38134=CARTESIAN_POINT('',(13.2026107084364,37.03,-18.990946838509));
#38135=CARTESIAN_POINT('',(11.8841806942968,37.03,-19.2474024814435));
#38136=CARTESIAN_POINT('',(12.5300905656334,37.03,-19.1013106159343));
#38137=CARTESIAN_POINT('',(11.2673077173324,37.03,-19.428591225812));
#38138=CARTESIAN_POINT('',(11.8841806942968,37.03,-19.2474024814435));
#38139=CARTESIAN_POINT('',(10.6822399290158,37.03,-19.6444956527339));
#38140=CARTESIAN_POINT('',(11.2673077173324,37.03,-19.428591225812));
#38141=CARTESIAN_POINT('',(10.1323656482948,37.03,-19.8951910916424));
#38142=CARTESIAN_POINT('',(10.6822399290158,37.03,-19.6444956527339));
#38143=CARTESIAN_POINT('',(10.0758530134688,37.03,-19.9269309927904));
#38144=CARTESIAN_POINT('',(10.1323656482948,37.03,-19.8951910916424));
#38145=CARTESIAN_POINT('',(8.07719355673392,37.03,-22.6893191554432));
#38146=CARTESIAN_POINT('',(4.23360628809444,37.03,-28.001619826393));
#38147=CARTESIAN_POINT('',(6.53125,37.03,-21.6875431630658));
#38148=CARTESIAN_POINT('',(7.65703498052716,37.03,-22.4170551566691));
#38149=CARTESIAN_POINT('',(4.8907147633328,37.03,-20.8496047663061));
#38150=CARTESIAN_POINT('',(6.53125,37.03,-21.6875431630658));
#38151=CARTESIAN_POINT('',(6.28368335893611,37.03,-17.7375208219333));
#38152=CARTESIAN_POINT('',(2.59831581724435,37.03,-25.9711401524854));
#38153=CARTESIAN_POINT('',(6.28291460223091,37.03,-17.6727094939652));
#38154=CARTESIAN_POINT('',(6.28985303478256,37.03,-18.2576657286835));
#38155=CARTESIAN_POINT('',(6.22508608057805,37.03,-17.0711566785188));
#38156=CARTESIAN_POINT('',(6.28291460223091,37.03,-17.6727094939652));
#38157=CARTESIAN_POINT('',(6.11953090492364,37.03,-16.4565208974396));
#38158=CARTESIAN_POINT('',(6.22508608057805,37.03,-17.0711566785188));
#38159=CARTESIAN_POINT('',(5.96800847194436,37.03,-15.8316988562961));
#38160=CARTESIAN_POINT('',(6.11953090492364,37.03,-16.4565208974396));
#38161=CARTESIAN_POINT('',(5.77157280309329,37.03,-15.1992785664089));
#38162=CARTESIAN_POINT('',(5.96800847194436,37.03,-15.8316988562961));
#38163=CARTESIAN_POINT('',(5.53089056659976,37.03,-14.5616771494721));
#38164=CARTESIAN_POINT('',(5.77157280309329,37.03,-15.1992785664089));
#38165=CARTESIAN_POINT('',(5.25715540570603,37.03,-14.481770682912));
#38166=CARTESIAN_POINT('',(5.53089056659976,37.03,-14.5616771494721));
#38167=CARTESIAN_POINT('',(4.98226661822352,37.03,-14.4059278439354));
#38168=CARTESIAN_POINT('',(5.25715540570603,37.03,-14.481770682912));
#38169=CARTESIAN_POINT('',(4.70628452555987,37.03,-14.3341652754431));
#38170=CARTESIAN_POINT('',(4.98226661822352,37.03,-14.4059278439354));
#38171=CARTESIAN_POINT('',(4.42926968903683,37.03,-14.2664987249639));
#38172=CARTESIAN_POINT('',(4.70628452555987,37.03,-14.3341652754431));
#38173=CARTESIAN_POINT('',(3.90203204952539,37.03,-14.6983366312733));
#38174=CARTESIAN_POINT('',(4.42926968903683,37.03,-14.2664987249639));
#38175=CARTESIAN_POINT('',(3.41570362514739,37.03,-15.1478108337588));
#38176=CARTESIAN_POINT('',(3.90203204952539,37.03,-14.6983366312733));
#38177=CARTESIAN_POINT('',(2.97207032837233,37.03,-15.6131613777439));
#38178=CARTESIAN_POINT('',(3.41570362514739,37.03,-15.1478108337588));
#38179=CARTESIAN_POINT('',(2.57333897421511,37.03,-16.0926739904062));
#38180=CARTESIAN_POINT('',(2.97207032837233,37.03,-15.6131613777439));
#38181=CARTESIAN_POINT('',(2.22248159767725,37.03,-16.5847197494743));
#38182=CARTESIAN_POINT('',(2.57333897421511,37.03,-16.0926739904062));
#38183=CARTESIAN_POINT('',(2.18941017085717,37.03,-16.6404636275951));
#38184=CARTESIAN_POINT('',(2.22248159767725,37.03,-16.5847197494743));
#38185=CARTESIAN_POINT('',(1.83971438913717,37.03,-20.0320916799333));
#38186=CARTESIAN_POINT('',(1.16722050830783,37.03,-26.5544726478367));
#38187=CARTESIAN_POINT('',(7.99847440693115E-16,37.03,-19.9375));
#38188=CARTESIAN_POINT('',(1.33971438913717,37.03,-20.0063834285624));
#38189=CARTESIAN_POINT('',(-1.83971438913717,37.03,-20.0320916799333));
#38190=CARTESIAN_POINT('',(7.99847440693115E-16,37.03,-19.9375));
#38191=CARTESIAN_POINT('',(-2.18941017085717,37.03,-16.6404636275951));
#38192=CARTESIAN_POINT('',(-1.26422241896876,37.03,-25.6136709037898));
#38193=CARTESIAN_POINT('',(-2.22248159767725,37.03,-16.5847197494743));
#38194=CARTESIAN_POINT('',(-1.92399462146589,37.03,-17.0878374925667));
#38195=CARTESIAN_POINT('',(-2.57333897421511,37.03,-16.0926739904062));
#38196=CARTESIAN_POINT('',(-2.22248159767725,37.03,-16.5847197494743));
#38197=CARTESIAN_POINT('',(-2.97207032837233,37.03,-15.6131613777439));
#38198=CARTESIAN_POINT('',(-2.57333897421511,37.03,-16.0926739904062));
#38199=CARTESIAN_POINT('',(-3.4157036251474,37.03,-15.1478108337588));
#38200=CARTESIAN_POINT('',(-2.97207032837233,37.03,-15.6131613777439));
#38201=CARTESIAN_POINT('',(-3.90203204952539,37.03,-14.6983366312733));
#38202=CARTESIAN_POINT('',(-3.4157036251474,37.03,-15.1478108337588));
#38203=CARTESIAN_POINT('',(-4.42926968903683,37.03,-14.2664987249639));
#38204=CARTESIAN_POINT('',(-3.90203204952539,37.03,-14.6983366312733));
#38205=CARTESIAN_POINT('',(-4.70628452555987,37.03,-14.3341652754431));
#38206=CARTESIAN_POINT('',(-4.42926968903683,37.03,-14.2664987249639));
#38207=CARTESIAN_POINT('',(-4.98226661822353,37.03,-14.4059278439354));
#38208=CARTESIAN_POINT('',(-4.70628452555987,37.03,-14.3341652754431));
#38209=CARTESIAN_POINT('',(-5.25715540570604,37.03,-14.481770682912));
#38210=CARTESIAN_POINT('',(-4.98226661822353,37.03,-14.4059278439354));
#38211=CARTESIAN_POINT('',(-5.53089056659977,37.03,-14.5616771494721));
#38212=CARTESIAN_POINT('',(-5.25715540570604,37.03,-14.481770682912));
#38213=CARTESIAN_POINT('',(-5.7715728030933,37.03,-15.1992785664089));
#38214=CARTESIAN_POINT('',(-5.53089056659977,37.03,-14.5616771494721));
#38215=CARTESIAN_POINT('',(-5.96800847194436,37.03,-15.8316988562961));
#38216=CARTESIAN_POINT('',(-5.7715728030933,37.03,-15.1992785664089));
#38217=CARTESIAN_POINT('',(-6.11953090492364,37.03,-16.4565208974396));
#38218=CARTESIAN_POINT('',(-5.96800847194436,37.03,-15.8316988562961));
#38219=CARTESIAN_POINT('',(-6.22508608057805,37.03,-17.0711566785188));
#38220=CARTESIAN_POINT('',(-6.11953090492364,37.03,-16.4565208974396));
#38221=CARTESIAN_POINT('',(-6.28291460223091,37.03,-17.6727094939652));
#38222=CARTESIAN_POINT('',(-6.22508608057805,37.03,-17.0711566785188));
#38223=CARTESIAN_POINT('',(-6.28368335893612,37.03,-17.7375208219333));
#38224=CARTESIAN_POINT('',(-6.28291460223091,37.03,-17.6727094939652));
#38225=CARTESIAN_POINT('',(-4.8907147633328,37.03,-20.8496047663061));
#38226=CARTESIAN_POINT('',(-2.21192106406889,37.03,-26.8343993180852));
#38227=CARTESIAN_POINT('',(-6.53125,37.03,-21.6875431630658));
#38228=CARTESIAN_POINT('',(-5.33658159091048,37.03,-21.077340767532));
#38229=CARTESIAN_POINT('',(-8.07719355673392,37.03,-22.6893191554432));
#38230=CARTESIAN_POINT('',(-6.53125,37.03,-21.6875431630658));
#38231=CARTESIAN_POINT('',(-10.0758530134688,37.03,-19.9269309927904));
#38232=CARTESIAN_POINT('',(-4.78801327896586,37.03,-27.2353625714542));
#38233=CARTESIAN_POINT('',(-10.1323656482948,37.03,-19.8951910916424));
#38234=CARTESIAN_POINT('',(-9.62230947265072,37.03,-20.1816603501494));
#38235=CARTESIAN_POINT('',(-10.6822399290158,37.03,-19.6444956527339));
#38236=CARTESIAN_POINT('',(-10.1323656482948,37.03,-19.8951910916424));
#38237=CARTESIAN_POINT('',(-11.2673077173324,37.03,-19.428591225812));
#38238=CARTESIAN_POINT('',(-10.6822399290158,37.03,-19.6444956527339));
#38239=CARTESIAN_POINT('',(-11.8841806942968,37.03,-19.2474024814435));
#38240=CARTESIAN_POINT('',(-11.2673077173324,37.03,-19.428591225812));
#38241=CARTESIAN_POINT('',(-12.5300905656334,37.03,-19.1013106159343));
#38242=CARTESIAN_POINT('',(-11.8841806942968,37.03,-19.2474024814435));
#38243=CARTESIAN_POINT('',(-13.2026107084363,37.03,-18.990946838509));
#38244=CARTESIAN_POINT('',(-12.5300905656334,37.03,-19.1013106159343));
#38245=CARTESIAN_POINT('',(-13.4086793188509,37.03,-19.1880552084719));
#38246=CARTESIAN_POINT('',(-13.2026107084363,37.03,-18.990946838509));
#38247=CARTESIAN_POINT('',(-13.611805537841,37.03,-19.388194462159));
#38248=CARTESIAN_POINT('',(-13.4086793188509,37.03,-19.1880552084719));
#38249=CARTESIAN_POINT('',(-13.8119447915281,37.03,-19.5913206811491));
#38250=CARTESIAN_POINT('',(-13.611805537841,37.03,-19.388194462159));
#38251=CARTESIAN_POINT('',(-14.009053161491,37.03,-19.7973892915637));
#38252=CARTESIAN_POINT('',(-13.8119447915281,37.03,-19.5913206811491));
#38253=CARTESIAN_POINT('',(-13.8986893840657,37.03,-20.4699094343666));
#38254=CARTESIAN_POINT('',(-14.009053161491,37.03,-19.7973892915637));
#38255=CARTESIAN_POINT('',(-13.7525975185565,37.03,-21.1158193057032));
#38256=CARTESIAN_POINT('',(-13.8986893840657,37.03,-20.4699094343666));
#38257=CARTESIAN_POINT('',(-13.571408774188,37.03,-21.7326922826676));
#38258=CARTESIAN_POINT('',(-13.7525975185565,37.03,-21.1158193057032));
#38259=CARTESIAN_POINT('',(-13.3555043472661,37.03,-22.3177600709842));
#38260=CARTESIAN_POINT('',(-13.571408774188,37.03,-21.7326922826676));
#38261=CARTESIAN_POINT('',(-13.1048089083576,37.03,-22.8676343517052));
#38262=CARTESIAN_POINT('',(-13.3555043472661,37.03,-22.3177600709842));
#38263=CARTESIAN_POINT('',(-13.0730690072096,37.03,-22.9241469865312));
#38264=CARTESIAN_POINT('',(-13.1048089083576,37.03,-22.8676343517052));
#38265=CARTESIAN_POINT('',(-10.3106808445568,37.03,-24.9228064432661));
#38266=CARTESIAN_POINT('',(-4.99838017360698,37.03,-28.7663937119056));
#38267=CARTESIAN_POINT('',(-11.3124568369342,37.03,-26.46875));
#38268=CARTESIAN_POINT('',(-10.5829448433309,37.03,-25.3429650194728));
#38269=CARTESIAN_POINT('',(-12.1503952336939,37.03,-28.1092852366672));
#38270=CARTESIAN_POINT('',(-11.3124568369342,37.03,-26.46875));
#38271=CARTESIAN_POINT('',(-15.2624791780667,37.03,-26.7163166410639));
#38272=CARTESIAN_POINT('',(-7.02885984751459,37.03,-30.4016841827556));
#38273=CARTESIAN_POINT('',(-15.3272905060348,37.03,-26.7170853977691));
#38274=CARTESIAN_POINT('',(-14.7423342713164,37.03,-26.7101469652174));
#38275=CARTESIAN_POINT('',(-15.9288433214812,37.03,-26.7749139194219));
#38276=CARTESIAN_POINT('',(-15.3272905060348,37.03,-26.7170853977691));
#38277=CARTESIAN_POINT('',(-16.5434791025604,37.03,-26.8804690950764));
#38278=CARTESIAN_POINT('',(-15.9288433214812,37.03,-26.7749139194219));
#38279=CARTESIAN_POINT('',(-17.1683011437039,37.03,-27.0319915280556));
#38280=CARTESIAN_POINT('',(-16.5434791025604,37.03,-26.8804690950764));
#38281=CARTESIAN_POINT('',(-17.8007214335911,37.03,-27.2284271969067));
#38282=CARTESIAN_POINT('',(-17.1683011437039,37.03,-27.0319915280556));
#38283=CARTESIAN_POINT('',(-18.4383228505279,37.03,-27.4691094334002));
#38284=CARTESIAN_POINT('',(-17.8007214335911,37.03,-27.2284271969067));
#38285=CARTESIAN_POINT('',(-18.518229317088,37.03,-27.742844594294));
#38286=CARTESIAN_POINT('',(-18.4383228505279,37.03,-27.4691094334002));
#38287=CARTESIAN_POINT('',(-18.5940721560646,37.03,-28.0177333817765));
#38288=CARTESIAN_POINT('',(-18.518229317088,37.03,-27.742844594294));
#38289=CARTESIAN_POINT('',(-18.6658347245569,37.03,-28.2937154744401));
#38290=CARTESIAN_POINT('',(-18.5940721560646,37.03,-28.0177333817765));
#38291=CARTESIAN_POINT('',(-18.7335012750361,37.03,-28.5707303109632));
#38292=CARTESIAN_POINT('',(-18.6658347245569,37.03,-28.2937154744401));
#38293=CARTESIAN_POINT('',(-18.3016633687267,37.03,-29.0979679504746));
#38294=CARTESIAN_POINT('',(-18.7335012750361,37.03,-28.5707303109632));
#38295=CARTESIAN_POINT('',(-17.8521891662412,37.03,-29.5842963748526));
#38296=CARTESIAN_POINT('',(-18.3016633687267,37.03,-29.0979679504746));
#38297=CARTESIAN_POINT('',(-17.3868386222561,37.03,-30.0279296716277));
#38298=CARTESIAN_POINT('',(-17.8521891662412,37.03,-29.5842963748526));
#38299=CARTESIAN_POINT('',(-16.9073260095938,37.03,-30.4266610257849));
#38300=CARTESIAN_POINT('',(-17.3868386222561,37.03,-30.0279296716277));
#38301=CARTESIAN_POINT('',(-16.4152802505257,37.03,-30.7775184023227));
#38302=CARTESIAN_POINT('',(-16.9073260095938,37.03,-30.4266610257849));
#38303=CARTESIAN_POINT('',(-16.3595363724049,37.03,-30.8105898291428));
#38304=CARTESIAN_POINT('',(-16.4152802505257,37.03,-30.7775184023227));
#38305=CARTESIAN_POINT('',(-12.9679083200667,37.03,-31.1602856108628));
#38306=CARTESIAN_POINT('',(-6.44552735216333,37.03,-31.8327794916922));
#38307=CARTESIAN_POINT('',(-13.0625,37.03,-33.));
#38308=CARTESIAN_POINT('',(-12.9936165714376,37.03,-31.6602856108628));
#38309=CARTESIAN_POINT('',(-12.9679083200667,37.03,-34.8397143891372));
#38310=CARTESIAN_POINT('',(-13.0625,37.03,-33.));
#38311=CARTESIAN_POINT('',(-16.3595363724049,37.03,-35.1894101708572));
#38312=CARTESIAN_POINT('',(-7.38632909621023,37.03,-34.2642224189688));
#38313=CARTESIAN_POINT('',(-16.4152802505257,37.03,-35.2224815976773));
#38314=CARTESIAN_POINT('',(-15.9121625074333,37.03,-34.9239946214659));
#38315=CARTESIAN_POINT('',(-16.9073260095938,37.03,-35.5733389742151));
#38316=CARTESIAN_POINT('',(-16.4152802505257,37.03,-35.2224815976773));
#38317=CARTESIAN_POINT('',(-17.3868386222561,37.03,-35.9720703283723));
#38318=CARTESIAN_POINT('',(-16.9073260095938,37.03,-35.5733389742151));
#38319=CARTESIAN_POINT('',(-17.8521891662412,37.03,-36.4157036251474));
#38320=CARTESIAN_POINT('',(-17.3868386222561,37.03,-35.9720703283723));
#38321=CARTESIAN_POINT('',(-18.3016633687267,37.03,-36.9020320495254));
#38322=CARTESIAN_POINT('',(-17.8521891662412,37.03,-36.4157036251474));
#38323=CARTESIAN_POINT('',(-18.7335012750361,37.03,-37.4292696890368));
#38324=CARTESIAN_POINT('',(-18.3016633687267,37.03,-36.9020320495254));
#38325=CARTESIAN_POINT('',(-18.6658347245569,37.03,-37.7062845255599));
#38326=CARTESIAN_POINT('',(-18.7335012750361,37.03,-37.4292696890368));
#38327=CARTESIAN_POINT('',(-18.5940721560646,37.03,-37.9822666182235));
#38328=CARTESIAN_POINT('',(-18.6658347245569,37.03,-37.7062845255599));
#38329=CARTESIAN_POINT('',(-18.518229317088,37.03,-38.257155405706));
#38330=CARTESIAN_POINT('',(-18.5940721560646,37.03,-37.9822666182235));
#38331=CARTESIAN_POINT('',(-18.4383228505279,37.03,-38.5308905665998));
#38332=CARTESIAN_POINT('',(-18.518229317088,37.03,-38.257155405706));
#38333=CARTESIAN_POINT('',(-17.8007214335911,37.03,-38.7715728030933));
#38334=CARTESIAN_POINT('',(-18.4383228505279,37.03,-38.5308905665998));
#38335=CARTESIAN_POINT('',(-17.1683011437039,37.03,-38.9680084719444));
#38336=CARTESIAN_POINT('',(-17.8007214335911,37.03,-38.7715728030933));
#38337=CARTESIAN_POINT('',(-16.5434791025604,37.03,-39.1195309049236));
#38338=CARTESIAN_POINT('',(-17.1683011437039,37.03,-38.9680084719444));
#38339=CARTESIAN_POINT('',(-15.9288433214812,37.03,-39.225086080578));
#38340=CARTESIAN_POINT('',(-16.5434791025604,37.03,-39.1195309049236));
#38341=CARTESIAN_POINT('',(-15.3272905060348,37.03,-39.2829146022309));
#38342=CARTESIAN_POINT('',(-15.9288433214812,37.03,-39.225086080578));
#38343=CARTESIAN_POINT('',(-15.2624791780667,37.03,-39.2836833589361));
#38344=CARTESIAN_POINT('',(-15.3272905060348,37.03,-39.2829146022309));
#38345=CARTESIAN_POINT('',(-12.1503952336939,37.03,-37.8907147633328));
#38346=CARTESIAN_POINT('',(-6.16560068191481,37.03,-35.2119210640689));
#38347=CARTESIAN_POINT('',(-11.3124568369342,37.03,-39.53125));
#38348=CARTESIAN_POINT('',(-11.922659232468,37.03,-38.3365815909105));
#38349=CARTESIAN_POINT('',(-10.3106808445568,37.03,-41.0771935567339));
#38350=CARTESIAN_POINT('',(-11.3124568369342,37.03,-39.53125));
#38351=CARTESIAN_POINT('',(-13.0730690072096,37.03,-43.0758530134688));
#38352=CARTESIAN_POINT('',(-5.76463742854584,37.03,-37.7880132789659));
#38353=CARTESIAN_POINT('',(-13.1048089083576,37.03,-43.1323656482948));
#38354=CARTESIAN_POINT('',(-12.8183396498506,37.03,-42.6223094726507));
#38355=CARTESIAN_POINT('',(-13.3555043472661,37.03,-43.6822399290158));
#38356=CARTESIAN_POINT('',(-13.1048089083576,37.03,-43.1323656482948));
#38357=CARTESIAN_POINT('',(-13.571408774188,37.03,-44.2673077173324));
#38358=CARTESIAN_POINT('',(-13.3555043472661,37.03,-43.6822399290158));
#38359=CARTESIAN_POINT('',(-13.7525975185565,37.03,-44.8841806942968));
#38360=CARTESIAN_POINT('',(-13.571408774188,37.03,-44.2673077173324));
#38361=CARTESIAN_POINT('',(-13.8986893840657,37.03,-45.5300905656334));
#38362=CARTESIAN_POINT('',(-13.7525975185565,37.03,-44.8841806942968));
#38363=CARTESIAN_POINT('',(-14.009053161491,37.03,-46.2026107084363));
#38364=CARTESIAN_POINT('',(-13.8986893840657,37.03,-45.5300905656334));
#38365=CARTESIAN_POINT('',(-13.8119447915281,37.03,-46.4086793188509));
#38366=CARTESIAN_POINT('',(-14.009053161491,37.03,-46.2026107084363));
#38367=CARTESIAN_POINT('',(-13.611805537841,37.03,-46.611805537841));
#38368=CARTESIAN_POINT('',(-13.8119447915281,37.03,-46.4086793188509));
#38369=CARTESIAN_POINT('',(-13.4086793188509,37.03,-46.8119447915281));
#38370=CARTESIAN_POINT('',(-13.611805537841,37.03,-46.611805537841));
#38371=CARTESIAN_POINT('',(-13.2026107084363,37.03,-47.009053161491));
#38372=CARTESIAN_POINT('',(-13.4086793188509,37.03,-46.8119447915281));
#38373=CARTESIAN_POINT('',(-12.5300905656334,37.03,-46.8986893840657));
#38374=CARTESIAN_POINT('',(-13.2026107084363,37.03,-47.009053161491));
#38375=CARTESIAN_POINT('',(-11.8841806942968,37.03,-46.7525975185565));
#38376=CARTESIAN_POINT('',(-12.5300905656334,37.03,-46.8986893840657));
#38377=CARTESIAN_POINT('',(-11.2673077173324,37.03,-46.571408774188));
#38378=CARTESIAN_POINT('',(-11.8841806942968,37.03,-46.7525975185565));
#38379=CARTESIAN_POINT('',(-10.6822399290158,37.03,-46.3555043472661));
#38380=CARTESIAN_POINT('',(-11.2673077173324,37.03,-46.571408774188));
#38381=CARTESIAN_POINT('',(-10.1323656482948,37.03,-46.1048089083576));
#38382=CARTESIAN_POINT('',(-10.6822399290158,37.03,-46.3555043472661));
#38383=CARTESIAN_POINT('',(-10.0758530134688,37.03,-46.0730690072096));
#38384=CARTESIAN_POINT('',(-10.1323656482948,37.03,-46.1048089083576));
#38385=CARTESIAN_POINT('',(-8.07719355673392,37.03,-43.3106808445568));
#38386=CARTESIAN_POINT('',(-4.23360628809444,37.03,-37.998380173607));
#38387=CARTESIAN_POINT('',(-6.53125000000001,37.03,-44.3124568369342));
#38388=CARTESIAN_POINT('',(-7.65703498052716,37.03,-43.5829448433309));
#38389=CARTESIAN_POINT('',(-4.8907147633328,37.03,-45.1503952336939));
#38390=CARTESIAN_POINT('',(-6.53125000000001,37.03,-44.3124568369342));
#38391=CARTESIAN_POINT('',(-6.2836833589361,37.03,-48.2624791780667));
#38392=CARTESIAN_POINT('',(-2.59831581724436,37.03,-40.0288598475146));
#38393=CARTESIAN_POINT('',(-6.2829146022309,37.03,-48.3272905060348));
#38394=CARTESIAN_POINT('',(-6.28985303478255,37.03,-47.7423342713165));
#38395=CARTESIAN_POINT('',(-6.22508608057804,37.03,-48.9288433214812));
#38396=CARTESIAN_POINT('',(-6.2829146022309,37.03,-48.3272905060348));
#38397=CARTESIAN_POINT('',(-6.11953090492364,37.03,-49.5434791025604));
#38398=CARTESIAN_POINT('',(-6.22508608057804,37.03,-48.9288433214812));
#38399=CARTESIAN_POINT('',(-5.96800847194436,37.03,-50.1683011437039));
#38400=CARTESIAN_POINT('',(-6.11953090492364,37.03,-49.5434791025604));
#38401=CARTESIAN_POINT('',(-5.7715728030933,37.03,-50.8007214335911));
#38402=CARTESIAN_POINT('',(-5.96800847194436,37.03,-50.1683011437039));
#38403=CARTESIAN_POINT('',(-5.53089056659976,37.03,-51.4383228505279));
#38404=CARTESIAN_POINT('',(-5.7715728030933,37.03,-50.8007214335911));
#38405=CARTESIAN_POINT('',(-5.25715540570604,37.03,-51.518229317088));
#38406=CARTESIAN_POINT('',(-5.53089056659976,37.03,-51.4383228505279));
#38407=CARTESIAN_POINT('',(-4.98226661822352,37.03,-51.5940721560646));
#38408=CARTESIAN_POINT('',(-5.25715540570604,37.03,-51.518229317088));
#38409=CARTESIAN_POINT('',(-4.70628452555985,37.03,-51.6658347245569));
#38410=CARTESIAN_POINT('',(-4.98226661822352,37.03,-51.5940721560646));
#38411=CARTESIAN_POINT('',(-4.42926968903682,37.03,-51.7335012750361));
#38412=CARTESIAN_POINT('',(-4.70628452555985,37.03,-51.6658347245569));
#38413=CARTESIAN_POINT('',(-3.90203204952539,37.03,-51.3016633687267));
#38414=CARTESIAN_POINT('',(-4.42926968903682,37.03,-51.7335012750361));
#38415=CARTESIAN_POINT('',(-3.41570362514739,37.03,-50.8521891662412));
#38416=CARTESIAN_POINT('',(-3.90203204952539,37.03,-51.3016633687267));
#38417=CARTESIAN_POINT('',(-2.97207032837234,37.03,-50.3868386222561));
#38418=CARTESIAN_POINT('',(-3.41570362514739,37.03,-50.8521891662412));
#38419=CARTESIAN_POINT('',(-2.57333897421511,37.03,-49.9073260095938));
#38420=CARTESIAN_POINT('',(-2.97207032837234,37.03,-50.3868386222561));
#38421=CARTESIAN_POINT('',(-2.22248159767726,37.03,-49.4152802505257));
#38422=CARTESIAN_POINT('',(-2.57333897421511,37.03,-49.9073260095938));
#38423=CARTESIAN_POINT('',(-2.18941017085716,37.03,-49.3595363724049));
#38424=CARTESIAN_POINT('',(-2.22248159767726,37.03,-49.4152802505257));
#38425=CARTESIAN_POINT('',(-1.83971438913717,37.03,-45.9679083200667));
#38426=CARTESIAN_POINT('',(-1.16722050830782,37.03,-39.4455273521633));
#38427=CARTESIAN_POINT('',(-2.39954232207934E-15,37.03,-46.0625));
#38428=CARTESIAN_POINT('',(-1.33971438913717,37.03,-45.9936165714376));
#38429=CARTESIAN_POINT('',(1.83971438913716,37.03,-45.9679083200667));
#38430=CARTESIAN_POINT('',(-2.39954232207934E-15,37.03,-46.0625));
#38431=CARTESIAN_POINT('',(2.18941017085715,37.03,-49.3595363724049));
#38432=CARTESIAN_POINT('',(1.26422241896875,37.03,-40.3863290962102));
#38433=CARTESIAN_POINT('',(2.22248159767725,37.03,-49.4152802505257));
#38434=CARTESIAN_POINT('',(1.92399462146588,37.03,-48.9121625074333));
#38435=CARTESIAN_POINT('',(2.57333897421511,37.03,-49.9073260095938));
#38436=CARTESIAN_POINT('',(2.22248159767725,37.03,-49.4152802505257));
#38437=CARTESIAN_POINT('',(2.97207032837233,37.03,-50.3868386222561));
#38438=CARTESIAN_POINT('',(2.57333897421511,37.03,-49.9073260095938));
#38439=CARTESIAN_POINT('',(3.41570362514738,37.03,-50.8521891662412));
#38440=CARTESIAN_POINT('',(2.97207032837233,37.03,-50.3868386222561));
#38441=CARTESIAN_POINT('',(3.90203204952538,37.03,-51.3016633687267));
#38442=CARTESIAN_POINT('',(3.41570362514738,37.03,-50.8521891662412));
#38443=CARTESIAN_POINT('',(4.42926968903682,37.03,-51.7335012750361));
#38444=CARTESIAN_POINT('',(3.90203204952538,37.03,-51.3016633687267));
#38445=CARTESIAN_POINT('',(4.70628452555985,37.03,-51.6658347245569));
#38446=CARTESIAN_POINT('',(4.42926968903682,37.03,-51.7335012750361));
#38447=CARTESIAN_POINT('',(4.98226661822352,37.03,-51.5940721560646));
#38448=CARTESIAN_POINT('',(4.70628452555985,37.03,-51.6658347245569));
#38449=CARTESIAN_POINT('',(5.25715540570603,37.03,-51.518229317088));
#38450=CARTESIAN_POINT('',(4.98226661822352,37.03,-51.5940721560646));
#38451=CARTESIAN_POINT('',(5.53089056659975,37.03,-51.4383228505279));
#38452=CARTESIAN_POINT('',(5.25715540570603,37.03,-51.518229317088));
#38453=CARTESIAN_POINT('',(5.77157280309329,37.03,-50.8007214335911));
#38454=CARTESIAN_POINT('',(5.53089056659975,37.03,-51.4383228505279));
#38455=CARTESIAN_POINT('',(5.96800847194436,37.03,-50.1683011437039));
#38456=CARTESIAN_POINT('',(5.77157280309329,37.03,-50.8007214335911));
#38457=CARTESIAN_POINT('',(6.11953090492363,37.03,-49.5434791025604));
#38458=CARTESIAN_POINT('',(5.96800847194436,37.03,-50.1683011437039));
#38459=CARTESIAN_POINT('',(6.22508608057804,37.03,-48.9288433214812));
#38460=CARTESIAN_POINT('',(6.11953090492363,37.03,-49.5434791025604));
#38461=CARTESIAN_POINT('',(6.2829146022309,37.03,-48.3272905060348));
#38462=CARTESIAN_POINT('',(6.22508608057804,37.03,-48.9288433214812));
#38463=CARTESIAN_POINT('',(6.2836833589361,37.03,-48.2624791780667));
#38464=CARTESIAN_POINT('',(6.2829146022309,37.03,-48.3272905060348));
#38465=CARTESIAN_POINT('',(4.89071476333279,37.03,-45.1503952336939));
#38466=CARTESIAN_POINT('',(2.2119210640689,37.03,-39.1656006819148));
#38467=CARTESIAN_POINT('',(6.53125,37.03,-44.3124568369342));
#38468=CARTESIAN_POINT('',(5.33658159091047,37.03,-44.922659232468));
#38469=CARTESIAN_POINT('',(8.07719355673392,37.03,-43.3106808445568));
#38470=CARTESIAN_POINT('',(6.53125,37.03,-44.3124568369342));
#38471=CARTESIAN_POINT('',(10.0758530134688,37.03,-46.0730690072096));
#38472=CARTESIAN_POINT('',(4.78801327896586,37.03,-38.7646374285458));
#38473=CARTESIAN_POINT('',(10.1323656482948,37.03,-46.1048089083576));
#38474=CARTESIAN_POINT('',(9.62230947265071,37.03,-45.8183396498506));
#38475=CARTESIAN_POINT('',(10.6822399290158,37.03,-46.3555043472661));
#38476=CARTESIAN_POINT('',(10.1323656482948,37.03,-46.1048089083576));
#38477=CARTESIAN_POINT('',(11.2673077173324,37.03,-46.571408774188));
#38478=CARTESIAN_POINT('',(10.6822399290158,37.03,-46.3555043472661));
#38479=CARTESIAN_POINT('',(11.8841806942968,37.03,-46.7525975185565));
#38480=CARTESIAN_POINT('',(11.2673077173324,37.03,-46.571408774188));
#38481=CARTESIAN_POINT('',(12.5300905656334,37.03,-46.8986893840657));
#38482=CARTESIAN_POINT('',(11.8841806942968,37.03,-46.7525975185565));
#38483=CARTESIAN_POINT('',(13.2026107084363,37.03,-47.009053161491));
#38484=CARTESIAN_POINT('',(12.5300905656334,37.03,-46.8986893840657));
#38485=CARTESIAN_POINT('',(13.4086793188509,37.03,-46.8119447915281));
#38486=CARTESIAN_POINT('',(13.2026107084363,37.03,-47.009053161491));
#38487=CARTESIAN_POINT('',(13.611805537841,37.03,-46.6118055378411));
#38488=CARTESIAN_POINT('',(13.4086793188509,37.03,-46.8119447915281));
#38489=CARTESIAN_POINT('',(13.8119447915281,37.03,-46.4086793188509));
#38490=CARTESIAN_POINT('',(13.611805537841,37.03,-46.6118055378411));
#38491=CARTESIAN_POINT('',(14.009053161491,37.03,-46.2026107084364));
#38492=CARTESIAN_POINT('',(13.8119447915281,37.03,-46.4086793188509));
#38493=CARTESIAN_POINT('',(13.8986893840657,37.03,-45.5300905656334));
#38494=CARTESIAN_POINT('',(14.009053161491,37.03,-46.2026107084364));
#38495=CARTESIAN_POINT('',(13.7525975185565,37.03,-44.8841806942968));
#38496=CARTESIAN_POINT('',(13.8986893840657,37.03,-45.5300905656334));
#38497=CARTESIAN_POINT('',(13.571408774188,37.03,-44.2673077173324));
#38498=CARTESIAN_POINT('',(13.7525975185565,37.03,-44.8841806942968));
#38499=CARTESIAN_POINT('',(13.3555043472661,37.03,-43.6822399290158));
#38500=CARTESIAN_POINT('',(13.571408774188,37.03,-44.2673077173324));
#38501=CARTESIAN_POINT('',(13.1048089083576,37.03,-43.1323656482948));
#38502=CARTESIAN_POINT('',(13.3555043472661,37.03,-43.6822399290158));
#38503=CARTESIAN_POINT('',(13.0730690072096,37.03,-43.0758530134688));
#38504=CARTESIAN_POINT('',(13.1048089083576,37.03,-43.1323656482948));
#38505=CARTESIAN_POINT('',(10.3106808445568,37.03,-41.0771935567339));
#38506=CARTESIAN_POINT('',(4.99838017360697,37.03,-37.2336062880944));
#38507=CARTESIAN_POINT('',(11.3124568369342,37.03,-39.53125));
#38508=CARTESIAN_POINT('',(10.5829448433309,37.03,-40.6570349805272));
#38509=CARTESIAN_POINT('',(12.1503952336939,37.03,-37.8907147633328));
#38510=CARTESIAN_POINT('',(11.3124568369342,37.03,-39.53125));
#38511=CARTESIAN_POINT('',(15.2624791780667,37.03,-39.2836833589361));
#38512=CARTESIAN_POINT('',(7.02885984751459,37.03,-35.5983158172444));
#38513=CARTESIAN_POINT('',(15.3272905060348,37.03,-39.2829146022309));
#38514=CARTESIAN_POINT('',(14.7423342713165,37.03,-39.2898530347825));
#38515=CARTESIAN_POINT('',(15.9288433214812,37.03,-39.225086080578));
#38516=CARTESIAN_POINT('',(15.3272905060348,37.03,-39.2829146022309));
#38517=CARTESIAN_POINT('',(16.5434791025604,37.03,-39.1195309049236));
#38518=CARTESIAN_POINT('',(15.9288433214812,37.03,-39.225086080578));
#38519=CARTESIAN_POINT('',(17.1683011437039,37.03,-38.9680084719444));
#38520=CARTESIAN_POINT('',(16.5434791025604,37.03,-39.1195309049236));
#38521=CARTESIAN_POINT('',(17.8007214335911,37.03,-38.7715728030933));
#38522=CARTESIAN_POINT('',(17.1683011437039,37.03,-38.9680084719444));
#38523=CARTESIAN_POINT('',(18.4383228505279,37.03,-38.5308905665998));
#38524=CARTESIAN_POINT('',(17.8007214335911,37.03,-38.7715728030933));
#38525=CARTESIAN_POINT('',(18.518229317088,37.03,-38.257155405706));
#38526=CARTESIAN_POINT('',(18.4383228505279,37.03,-38.5308905665998));
#38527=CARTESIAN_POINT('',(18.5940721560646,37.03,-37.9822666182235));
#38528=CARTESIAN_POINT('',(18.518229317088,37.03,-38.257155405706));
#38529=CARTESIAN_POINT('',(18.6658347245569,37.03,-37.7062845255599));
#38530=CARTESIAN_POINT('',(18.5940721560646,37.03,-37.9822666182235));
#38531=CARTESIAN_POINT('',(18.7335012750361,37.03,-37.4292696890368));
#38532=CARTESIAN_POINT('',(18.6658347245569,37.03,-37.7062845255599));
#38533=CARTESIAN_POINT('',(18.3016633687267,37.03,-36.9020320495254));
#38534=CARTESIAN_POINT('',(18.7335012750361,37.03,-37.4292696890368));
#38535=CARTESIAN_POINT('',(17.8521891662412,37.03,-36.4157036251474));
#38536=CARTESIAN_POINT('',(18.3016633687267,37.03,-36.9020320495254));
#38537=CARTESIAN_POINT('',(17.3868386222561,37.03,-35.9720703283723));
#38538=CARTESIAN_POINT('',(17.8521891662412,37.03,-36.4157036251474));
#38539=CARTESIAN_POINT('',(16.9073260095938,37.03,-35.5733389742151));
#38540=CARTESIAN_POINT('',(17.3868386222561,37.03,-35.9720703283723));
#38541=CARTESIAN_POINT('',(16.4152802505257,37.03,-35.2224815976773));
#38542=CARTESIAN_POINT('',(16.9073260095938,37.03,-35.5733389742151));
#38543=CARTESIAN_POINT('',(16.3595363724049,37.03,-35.1894101708572));
#38544=CARTESIAN_POINT('',(16.4152802505257,37.03,-35.2224815976773));
#38545=CARTESIAN_POINT('',(12.9679083200667,37.03,-34.8397143891372));
#38546=CARTESIAN_POINT('',(6.44552735216333,37.03,-34.1672205083078));
#38547=CARTESIAN_POINT('',(13.0625,37.03,-33.));
#38548=CARTESIAN_POINT('',(12.9936165714376,37.03,-34.3397143891372));
#38549=CARTESIAN_POINT('',(12.9679083200667,37.03,-31.1602856108628));
#38550=CARTESIAN_POINT('',(13.0625,37.03,-33.));
#38551=CARTESIAN_POINT('',(16.3595363724049,37.03,-30.8105898291428));
#38552=CARTESIAN_POINT('',(7.38632909621023,37.03,-31.7357775810312));
#38553=CARTESIAN_POINT('',(16.4152802505257,37.03,-30.7775184023227));
#38554=CARTESIAN_POINT('',(15.9121625074333,37.03,-31.0760053785341));
#38555=CARTESIAN_POINT('',(16.9073260095938,37.03,-30.4266610257849));
#38556=CARTESIAN_POINT('',(16.4152802505257,37.03,-30.7775184023227));
#38557=CARTESIAN_POINT('',(17.3868386222561,37.03,-30.0279296716277));
#38558=CARTESIAN_POINT('',(16.9073260095938,37.03,-30.4266610257849));
#38559=CARTESIAN_POINT('',(17.8521891662412,37.03,-29.5842963748526));
#38560=CARTESIAN_POINT('',(17.3868386222561,37.03,-30.0279296716277));
#38561=CARTESIAN_POINT('',(18.3016633687267,37.03,-29.0979679504746));
#38562=CARTESIAN_POINT('',(17.8521891662412,37.03,-29.5842963748526));
#38563=CARTESIAN_POINT('',(18.7335012750361,37.03,-28.5707303109632));
#38564=CARTESIAN_POINT('',(18.3016633687267,37.03,-29.0979679504746));
#38565=CARTESIAN_POINT('',(18.6658347245569,37.03,-28.2937154744402));
#38566=CARTESIAN_POINT('',(18.7335012750361,37.03,-28.5707303109632));
#38567=CARTESIAN_POINT('',(18.5940721560646,37.03,-28.0177333817765));
#38568=CARTESIAN_POINT('',(18.6658347245569,37.03,-28.2937154744402));
#38569=CARTESIAN_POINT('',(18.518229317088,37.03,-27.742844594294));
#38570=CARTESIAN_POINT('',(18.5940721560646,37.03,-28.0177333817765));
#38571=CARTESIAN_POINT('',(18.4383228505279,37.03,-27.4691094334002));
#38572=CARTESIAN_POINT('',(18.518229317088,37.03,-27.742844594294));
#38573=CARTESIAN_POINT('',(17.8007214335911,37.03,-27.2284271969067));
#38574=CARTESIAN_POINT('',(18.4383228505279,37.03,-27.4691094334002));
#38575=CARTESIAN_POINT('',(17.1683011437039,37.03,-27.0319915280556));
#38576=CARTESIAN_POINT('',(17.8007214335911,37.03,-27.2284271969067));
#38577=CARTESIAN_POINT('',(16.5434791025604,37.03,-26.8804690950764));
#38578=CARTESIAN_POINT('',(17.1683011437039,37.03,-27.0319915280556));
#38579=CARTESIAN_POINT('',(15.9288433214812,37.03,-26.774913919422));
#38580=CARTESIAN_POINT('',(16.5434791025604,37.03,-26.8804690950764));
#38581=CARTESIAN_POINT('',(15.3272905060348,37.03,-26.7170853977691));
#38582=CARTESIAN_POINT('',(15.9288433214812,37.03,-26.774913919422));
#38583=CARTESIAN_POINT('',(15.2624791780667,37.03,-26.7163166410639));
#38584=CARTESIAN_POINT('',(15.3272905060348,37.03,-26.7170853977691));
#38585=CARTESIAN_POINT('',(12.1503952336939,37.03,-28.1092852366672));
#38586=CARTESIAN_POINT('',(6.1656006819148,37.03,-30.7880789359311));
#38587=CARTESIAN_POINT('',(11.922659232468,37.03,-27.6634184090895));
#38588=CARTESIAN_POINT('',(1.04094977927525E-15,37.03,-41.5));
#38589=CARTESIAN_POINT('Origin',(0.,37.03,-33.));
#38590=CARTESIAN_POINT('Origin',(13.1048089083576,37.03,-22.8676343517052));
#38591=CARTESIAN_POINT('',(12.8183396498506,64.7518675845618,-23.3776905273493));
#38592=CARTESIAN_POINT('',(12.8183396498506,37.03,-23.3776905273493));
#38593=CARTESIAN_POINT('',(13.0730690072096,64.97,-22.9241469865312));
#38594=CARTESIAN_POINT('',(8.8979438687676,61.3947146828798,-30.3579232040826));
#38595=CARTESIAN_POINT('',(13.1048089083576,64.97,-22.8676343517052));
#38596=CARTESIAN_POINT('',(12.8183396498506,64.97,-23.3776905273493));
#38597=CARTESIAN_POINT('',(13.1048089083576,37.03,-22.8676343517052));
#38598=CARTESIAN_POINT('Origin',(12.8183396498506,37.03,-23.3776905273493));
#38599=CARTESIAN_POINT('',(12.4929286389212,64.5678155074499,-23.8403088083181));
#38600=CARTESIAN_POINT('',(12.4929286389212,37.03,-23.8403088083181));
#38601=CARTESIAN_POINT('',(8.36376245460559,62.2323640708404,-29.7105089486481));
#38602=CARTESIAN_POINT('Origin',(7.41196956298798,37.28,-31.9844592379009));
#38603=CARTESIAN_POINT('',(15.9121625074333,37.2481324154382,-31.0760053785341));
#38604=CARTESIAN_POINT('',(13.3116513142512,38.5161005118285,-32.6188226083255));
#38605=CARTESIAN_POINT('',(12.9936165714376,37.53,-31.6602856108628));
#38606=CARTESIAN_POINT('',(12.984466051433,37.3520314584495,-31.4823170693123));
#38607=CARTESIAN_POINT('',(14.8752200595314,37.53,-31.466281789541));
#38608=CARTESIAN_POINT('',(7.43761002976572,37.53,-32.2331408947705));
#38609=CARTESIAN_POINT('',(15.3990391648128,37.4321844925501,-31.3139390566435));
#38610=CARTESIAN_POINT('',(11.7907769153056,38.1059743550985,-32.3633328770643));
#38611=CARTESIAN_POINT('',(12.6172283184415,38.429991495039,-32.603855985976));
#38612=CARTESIAN_POINT('Origin',(16.4152802505257,37.03,-30.7775184023227));
#38613=CARTESIAN_POINT('',(15.9121625074333,64.7518675845618,-31.0760053785341));
#38614=CARTESIAN_POINT('',(15.9121625074333,37.03,-31.0760053785341));
#38615=CARTESIAN_POINT('',(16.3595363724049,64.97,-30.8105898291428));
#38616=CARTESIAN_POINT('',(9.0268838297594,61.39471468288,-35.1608663103698));
#38617=CARTESIAN_POINT('',(16.4152802505257,64.97,-30.7775184023227));
#38618=CARTESIAN_POINT('',(15.9121625074333,64.97,-31.0760053785341));
#38619=CARTESIAN_POINT('',(16.4152802505257,37.03,-30.7775184023227));
#38620=CARTESIAN_POINT('Origin',(15.9121625074333,37.03,-31.0760053785341));
#38621=CARTESIAN_POINT('',(15.3990391648128,64.5678155074499,-31.3139390566435));
#38622=CARTESIAN_POINT('',(15.3990391648128,37.03,-31.3139390566435));
#38623=CARTESIAN_POINT('',(8.88797628258284,62.2323640708403,-34.3330984113106));
#38624=CARTESIAN_POINT('Origin',(6.9267243146742,37.28,-35.8265006829375));
#38625=CARTESIAN_POINT('',(14.7423342713165,37.2481324154382,-39.2898530347825));
#38626=CARTESIAN_POINT('',(11.7188169002993,38.5161005118285,-39.3257163525872));
#38627=CARTESIAN_POINT('',(11.922659232468,37.53,-38.3365815909105));
#38628=CARTESIAN_POINT('',(12.0037189204615,37.3520314584495,-38.177881052851));
#38629=CARTESIAN_POINT('',(13.6491775636676,37.53,-39.1093710972614));
#38630=CARTESIAN_POINT('',(6.82458878183381,37.53,-36.0546855486307));
#38631=CARTESIAN_POINT('',(14.1789895822776,37.4321844925501,-39.2393479731309));
#38632=CARTESIAN_POINT('',(10.5294459004776,38.1059743550985,-38.3440185554362));
#38633=CARTESIAN_POINT('',(11.1249122561308,38.429991495039,-38.9655433795188));
#38634=CARTESIAN_POINT('Origin',(15.3272905060348,37.03,-39.2829146022309));
#38635=CARTESIAN_POINT('',(14.7423342713165,64.7518675845618,-39.2898530347825));
#38636=CARTESIAN_POINT('',(14.7423342713165,37.03,-39.2898530347825));
#38637=CARTESIAN_POINT('',(15.2624791780667,64.97,-39.2836833589361));
#38638=CARTESIAN_POINT('',(6.73707755839776,61.3947146828801,-39.3848070338418));
#38639=CARTESIAN_POINT('',(15.3272905060348,64.97,-39.2829146022309));
#38640=CARTESIAN_POINT('',(14.7423342713165,64.97,-39.2898530347825));
#38641=CARTESIAN_POINT('',(15.3272905060348,37.03,-39.2829146022309));
#38642=CARTESIAN_POINT('Origin',(14.7423342713165,37.03,-39.2898530347825));
#38643=CARTESIAN_POINT('',(14.1789895822776,64.5678155074499,-39.2393479731309));
#38644=CARTESIAN_POINT('',(14.1789895822776,37.03,-39.2393479731309));
#38645=CARTESIAN_POINT('',(7.03066404329491,62.2323640708402,-38.5984852312312));
#38646=CARTESIAN_POINT('Origin',(4.58546888005044,37.28,-38.9111835525751));
#38647=CARTESIAN_POINT('',(9.62230947265071,37.2481324154382,-45.8183396498506));
#38648=CARTESIAN_POINT('',(6.98593496166402,38.5161005118286,-44.3376395086249));
#38649=CARTESIAN_POINT('',(7.65703498052716,37.53,-43.5829448433309));
#38650=CARTESIAN_POINT('',(7.80658499858209,37.3520314584495,-43.4860359897738));
#38651=CARTESIAN_POINT('',(8.76584896227005,37.53,-45.1154593532086));
#38652=CARTESIAN_POINT('',(4.38292448113502,37.53,-39.0577296766043));
#38653=CARTESIAN_POINT('',(9.15969119168186,37.4321844925501,-45.4929286389212));
#38654=CARTESIAN_POINT('',(6.44675835986946,38.1059743550985,-42.8927787775419));
#38655=CARTESIAN_POINT('',(6.65168493892267,38.4299914950389,-43.7287682421066));
#38656=CARTESIAN_POINT('Origin',(10.1323656482948,37.03,-46.1048089083576));
#38657=CARTESIAN_POINT('',(9.62230947265071,64.7518675845618,-45.8183396498506));
#38658=CARTESIAN_POINT('',(9.62230947265071,37.03,-45.8183396498506));
#38659=CARTESIAN_POINT('',(10.0758530134688,64.97,-46.0730690072096));
#38660=CARTESIAN_POINT('',(2.64207679591738,61.3947146828798,-41.8979438687676));
#38661=CARTESIAN_POINT('',(10.1323656482948,64.97,-46.1048089083576));
#38662=CARTESIAN_POINT('',(9.62230947265071,64.97,-45.8183396498506));
#38663=CARTESIAN_POINT('',(10.1323656482948,37.03,-46.1048089083576));
#38664=CARTESIAN_POINT('Origin',(9.62230947265071,37.03,-45.8183396498506));
#38665=CARTESIAN_POINT('',(9.15969119168186,64.5678155074499,-45.4929286389212));
#38666=CARTESIAN_POINT('',(9.15969119168186,37.03,-45.4929286389212));
#38667=CARTESIAN_POINT('',(3.2894910513519,62.2323640708404,-41.3637624546056));
#38668=CARTESIAN_POINT('Origin',(1.01554076209913,37.28,-40.411969562988));
#38669=CARTESIAN_POINT('',(1.92399462146588,37.2481324154382,-48.9121625074333));
#38670=CARTESIAN_POINT('',(0.381177391674463,38.5161005118285,-46.3116513142512));
#38671=CARTESIAN_POINT('',(1.33971438913717,37.53,-45.9936165714376));
#38672=CARTESIAN_POINT('',(1.51768293068769,37.3520314584495,-45.9844660514331));
#38673=CARTESIAN_POINT('',(1.53371821045902,37.53,-47.8752200595314));
#38674=CARTESIAN_POINT('',(0.766859105229514,37.53,-40.4376100297657));
#38675=CARTESIAN_POINT('',(1.68606094335647,37.4321844925501,-48.3990391648128));
#38676=CARTESIAN_POINT('',(0.636667122935676,38.1059743550985,-44.7907769153056));
#38677=CARTESIAN_POINT('',(0.396144014024024,38.429991495039,-45.6172283184415));
#38678=CARTESIAN_POINT('Origin',(2.22248159767725,37.03,-49.4152802505257));
#38679=CARTESIAN_POINT('',(1.92399462146588,64.7518675845618,-48.9121625074333));
#38680=CARTESIAN_POINT('',(1.92399462146588,37.03,-48.9121625074333));
#38681=CARTESIAN_POINT('',(2.18941017085715,64.97,-49.3595363724049));
#38682=CARTESIAN_POINT('',(-2.16086631036979,61.39471468288,-42.0268838297594));
#38683=CARTESIAN_POINT('',(2.22248159767725,64.97,-49.4152802505257));
#38684=CARTESIAN_POINT('',(1.92399462146588,64.97,-48.9121625074333));
#38685=CARTESIAN_POINT('',(2.22248159767725,37.03,-49.4152802505257));
#38686=CARTESIAN_POINT('Origin',(1.92399462146588,37.03,-48.9121625074333));
#38687=CARTESIAN_POINT('',(1.68606094335647,64.5678155074499,-48.3990391648128));
#38688=CARTESIAN_POINT('',(1.68606094335647,37.03,-48.3990391648128));
#38689=CARTESIAN_POINT('',(-1.3330984113107,62.2323640708402,-41.8879762825828));
#38690=CARTESIAN_POINT('Origin',(-2.82650068293752,37.28,-39.9267243146742));
#38691=CARTESIAN_POINT('',(-6.28985303478255,37.2481324154382,-47.7423342713165));
#38692=CARTESIAN_POINT('',(-6.32571635258722,38.5161005118285,-44.7188169002993));
#38693=CARTESIAN_POINT('',(-5.33658159091048,37.53,-44.922659232468));
#38694=CARTESIAN_POINT('',(-5.17788105285096,37.3520314584495,-45.0037189204615));
#38695=CARTESIAN_POINT('',(-6.10937109726139,37.53,-46.6491775636676));
#38696=CARTESIAN_POINT('',(-3.05468554863069,37.53,-39.8245887818338));
#38697=CARTESIAN_POINT('',(-6.23934797313094,37.4321844925501,-47.1789895822776));
#38698=CARTESIAN_POINT('',(-5.34401855543615,38.1059743550985,-43.5294459004776));
#38699=CARTESIAN_POINT('',(-5.96554337951879,38.429991495039,-44.1249122561308));
#38700=CARTESIAN_POINT('Origin',(-6.2829146022309,37.03,-48.3272905060348));
#38701=CARTESIAN_POINT('',(-6.28985303478255,64.7518675845618,-47.7423342713165));
#38702=CARTESIAN_POINT('',(-6.28985303478255,37.03,-47.7423342713165));
#38703=CARTESIAN_POINT('',(-6.2836833589361,64.97,-48.2624791780667));
#38704=CARTESIAN_POINT('',(-6.38480703384186,61.39471468288,-39.7370775583977));
#38705=CARTESIAN_POINT('',(-6.2829146022309,64.97,-48.3272905060348));
#38706=CARTESIAN_POINT('',(-6.28985303478255,64.97,-47.7423342713165));
#38707=CARTESIAN_POINT('',(-6.2829146022309,37.03,-48.3272905060348));
#38708=CARTESIAN_POINT('Origin',(-6.28985303478255,37.03,-47.7423342713165));
#38709=CARTESIAN_POINT('',(-6.23934797313094,64.5678155074499,-47.1789895822776));
#38710=CARTESIAN_POINT('',(-6.23934797313094,37.03,-47.1789895822776));
#38711=CARTESIAN_POINT('',(-5.59848523123113,62.2323640708402,-40.030664043295));
#38712=CARTESIAN_POINT('Origin',(-5.91118355257507,37.28,-37.5854688800504));
#38713=CARTESIAN_POINT('',(-12.8183396498506,37.2481324154382,-42.6223094726507));
#38714=CARTESIAN_POINT('',(-11.3376395086248,38.5161005118285,-39.985934961664));
#38715=CARTESIAN_POINT('',(-10.5829448433309,37.53,-40.6570349805272));
#38716=CARTESIAN_POINT('',(-10.4860359897738,37.3520314584495,-40.8065849985821));
#38717=CARTESIAN_POINT('',(-12.1154593532086,37.53,-41.76584896227));
#38718=CARTESIAN_POINT('',(-6.0577296766043,37.53,-37.382924481135));
#38719=CARTESIAN_POINT('',(-12.4929286389212,37.4321844925501,-42.1596911916819));
#38720=CARTESIAN_POINT('',(-9.89277877754201,38.1059743550986,-39.4467583598694));
#38721=CARTESIAN_POINT('',(-10.7287682421066,38.4299914950389,-39.6516849389227));
#38722=CARTESIAN_POINT('Origin',(-13.1048089083576,37.03,-43.1323656482948));
#38723=CARTESIAN_POINT('',(-12.8183396498506,64.7518675845618,-42.6223094726507));
#38724=CARTESIAN_POINT('',(-12.8183396498506,37.03,-42.6223094726507));
#38725=CARTESIAN_POINT('',(-13.0730690072096,64.97,-43.0758530134688));
#38726=CARTESIAN_POINT('',(-8.89794386876747,61.3947146828801,-35.6420767959176));
#38727=CARTESIAN_POINT('',(-13.1048089083576,64.97,-43.1323656482948));
#38728=CARTESIAN_POINT('',(-12.8183396498506,64.97,-42.6223094726507));
#38729=CARTESIAN_POINT('',(-13.1048089083576,37.03,-43.1323656482948));
#38730=CARTESIAN_POINT('Origin',(-12.8183396498506,37.03,-42.6223094726507));
#38731=CARTESIAN_POINT('',(-12.4929286389212,64.5678155074499,-42.1596911916819));
#38732=CARTESIAN_POINT('',(-12.4929286389212,37.03,-42.1596911916819));
#38733=CARTESIAN_POINT('',(-8.36376245460558,62.2323640708405,-36.289491051352));
#38734=CARTESIAN_POINT('Origin',(-7.41196956298797,37.28,-34.0155407620991));
#38735=CARTESIAN_POINT('',(-15.9121625074333,37.2481324154382,-34.9239946214659));
#38736=CARTESIAN_POINT('',(-13.3116513142512,38.5161005118285,-33.3811773916745));
#38737=CARTESIAN_POINT('',(-12.9936165714376,37.53,-34.3397143891372));
#38738=CARTESIAN_POINT('',(-12.984466051433,37.3520314584495,-34.5176829306877));
#38739=CARTESIAN_POINT('',(-14.8752200595314,37.53,-34.533718210459));
#38740=CARTESIAN_POINT('',(-7.43761002976572,37.53,-33.7668591052295));
#38741=CARTESIAN_POINT('',(-15.3990391648128,37.4321844925501,-34.6860609433565));
#38742=CARTESIAN_POINT('',(-11.7907769153057,38.1059743550986,-33.6366671229356));
#38743=CARTESIAN_POINT('',(-12.6172283184414,38.4299914950389,-33.3961440140241));
#38744=CARTESIAN_POINT('Origin',(-16.4152802505257,37.03,-35.2224815976773));
#38745=CARTESIAN_POINT('',(-15.9121625074333,64.7518675845618,-34.9239946214659));
#38746=CARTESIAN_POINT('',(-15.9121625074333,37.03,-34.9239946214659));
#38747=CARTESIAN_POINT('',(-16.3595363724049,64.97,-35.1894101708572));
#38748=CARTESIAN_POINT('',(-9.0268838297594,61.3947146828801,-30.8391336896303));
#38749=CARTESIAN_POINT('',(-16.4152802505257,64.97,-35.2224815976773));
#38750=CARTESIAN_POINT('',(-15.9121625074333,64.97,-34.9239946214659));
#38751=CARTESIAN_POINT('',(-16.4152802505257,37.03,-35.2224815976773));
#38752=CARTESIAN_POINT('Origin',(-15.9121625074333,37.03,-34.9239946214659));
#38753=CARTESIAN_POINT('',(-15.3990391648128,64.5678155074499,-34.6860609433565));
#38754=CARTESIAN_POINT('',(-15.3990391648128,37.03,-34.6860609433565));
#38755=CARTESIAN_POINT('',(-8.88797628258289,62.2323640708405,-31.6669015886896));
#38756=CARTESIAN_POINT('Origin',(-6.9267243146742,37.28,-30.1734993170625));
#38757=CARTESIAN_POINT('',(-14.7423342713164,37.2481324154382,-26.7101469652174));
#38758=CARTESIAN_POINT('',(-11.7188169002993,38.5161005118285,-26.6742836474128));
#38759=CARTESIAN_POINT('',(-11.922659232468,37.53,-27.6634184090895));
#38760=CARTESIAN_POINT('',(-12.0037189204615,37.3520314584495,-27.822118947149));
#38761=CARTESIAN_POINT('',(-13.6491775636676,37.53,-26.8906289027386));
#38762=CARTESIAN_POINT('',(-6.8245887818338,37.53,-29.9453144513693));
#38763=CARTESIAN_POINT('',(-14.1789895822776,37.4321844925501,-26.7606520268691));
#38764=CARTESIAN_POINT('',(-10.5294459004776,38.1059743550986,-27.6559814445638));
#38765=CARTESIAN_POINT('',(-11.1249122561307,38.4299914950389,-27.0344566204813));
#38766=CARTESIAN_POINT('Origin',(-15.3272905060348,37.03,-26.7170853977691));
#38767=CARTESIAN_POINT('',(-14.7423342713164,64.7518675845618,-26.7101469652174));
#38768=CARTESIAN_POINT('',(-14.7423342713164,37.03,-26.7101469652174));
#38769=CARTESIAN_POINT('',(-15.2624791780667,64.97,-26.7163166410639));
#38770=CARTESIAN_POINT('',(-6.73707755839773,61.39471468288,-26.6151929661581));
#38771=CARTESIAN_POINT('',(-15.3272905060348,64.97,-26.7170853977691));
#38772=CARTESIAN_POINT('',(-14.7423342713164,64.97,-26.7101469652174));
#38773=CARTESIAN_POINT('',(-15.3272905060348,37.03,-26.7170853977691));
#38774=CARTESIAN_POINT('Origin',(-14.7423342713164,37.03,-26.7101469652174));
#38775=CARTESIAN_POINT('',(-14.1789895822776,64.5678155074499,-26.7606520268691));
#38776=CARTESIAN_POINT('',(-14.1789895822776,37.03,-26.7606520268691));
#38777=CARTESIAN_POINT('',(-7.03066404329514,62.2323640708404,-27.401514768769));
#38778=CARTESIAN_POINT('Origin',(-4.58546888005044,37.28,-27.0888164474249));
#38779=CARTESIAN_POINT('',(-9.62230947265072,37.2481324154382,-20.1816603501494));
#38780=CARTESIAN_POINT('',(-6.98593496166398,38.5161005118285,-21.6623604913752));
#38781=CARTESIAN_POINT('',(-7.65703498052716,37.53,-22.4170551566691));
#38782=CARTESIAN_POINT('',(-7.80658499858209,37.3520314584495,-22.5139640102262));
#38783=CARTESIAN_POINT('',(-8.76584896227005,37.53,-20.8845406467914));
#38784=CARTESIAN_POINT('',(-4.38292448113502,37.53,-26.9422703233957));
#38785=CARTESIAN_POINT('',(-9.15969119168187,37.4321844925501,-20.5070713610788));
#38786=CARTESIAN_POINT('',(-6.44675835986946,38.1059743550986,-23.107221222458));
#38787=CARTESIAN_POINT('',(-6.65168493892268,38.4299914950389,-22.2712317578934));
#38788=CARTESIAN_POINT('Origin',(-10.1323656482948,37.03,-19.8951910916424));
#38789=CARTESIAN_POINT('',(-9.62230947265072,64.7518675845618,-20.1816603501494));
#38790=CARTESIAN_POINT('',(-9.62230947265072,37.03,-20.1816603501494));
#38791=CARTESIAN_POINT('',(-10.0758530134688,64.97,-19.9269309927904));
#38792=CARTESIAN_POINT('',(-2.64207679591758,61.39471468288,-24.1020561312325));
#38793=CARTESIAN_POINT('',(-10.1323656482948,64.97,-19.8951910916424));
#38794=CARTESIAN_POINT('',(-9.62230947265072,64.97,-20.1816603501494));
#38795=CARTESIAN_POINT('',(-10.1323656482948,37.03,-19.8951910916424));
#38796=CARTESIAN_POINT('Origin',(-9.62230947265072,37.03,-20.1816603501494));
#38797=CARTESIAN_POINT('',(-9.15969119168187,64.5678155074499,-20.5070713610788));
#38798=CARTESIAN_POINT('',(-9.15969119168187,37.03,-20.5070713610788));
#38799=CARTESIAN_POINT('',(-3.28949105135187,62.2323640708404,-24.6362375453944));
#38800=CARTESIAN_POINT('Origin',(-1.01554076209914,37.28,-25.588030437012));
#38801=CARTESIAN_POINT('',(-1.92399462146589,37.2481324154382,-17.0878374925667));
#38802=CARTESIAN_POINT('',(-0.381177391674473,38.5161005118285,-19.6883486857488));
#38803=CARTESIAN_POINT('',(-1.33971438913717,37.53,-20.0063834285624));
#38804=CARTESIAN_POINT('',(-1.5176829306877,37.3520314584495,-20.015533948567));
#38805=CARTESIAN_POINT('',(-1.53371821045904,37.53,-18.1247799404686));
#38806=CARTESIAN_POINT('',(-0.766859105229518,37.53,-25.5623899702343));
#38807=CARTESIAN_POINT('',(-1.68606094335648,37.4321844925501,-17.6009608351872));
#38808=CARTESIAN_POINT('',(-0.6366671229357,38.1059743550985,-21.2092230846944));
#38809=CARTESIAN_POINT('',(-0.396144014024061,38.4299914950389,-20.3827716815586));
#38810=CARTESIAN_POINT('Origin',(-2.22248159767725,37.03,-16.5847197494743));
#38811=CARTESIAN_POINT('',(-1.92399462146589,64.7518675845618,-17.0878374925667));
#38812=CARTESIAN_POINT('',(-1.92399462146589,37.03,-17.0878374925667));
#38813=CARTESIAN_POINT('',(-2.18941017085717,64.97,-16.6404636275951));
#38814=CARTESIAN_POINT('',(2.16086631036976,61.39471468288,-23.9731161702406));
#38815=CARTESIAN_POINT('',(-2.22248159767725,64.97,-16.5847197494743));
#38816=CARTESIAN_POINT('',(-1.92399462146589,64.97,-17.0878374925667));
#38817=CARTESIAN_POINT('',(-2.22248159767725,37.03,-16.5847197494743));
#38818=CARTESIAN_POINT('Origin',(-1.92399462146589,37.03,-17.0878374925667));
#38819=CARTESIAN_POINT('',(-1.68606094335648,64.5678155074499,-17.6009608351872));
#38820=CARTESIAN_POINT('',(-1.68606094335648,37.03,-17.6009608351872));
#38821=CARTESIAN_POINT('',(1.33309841131053,62.2323640708404,-24.1120237174171));
#38822=CARTESIAN_POINT('Origin',(2.82650068293752,37.28,-26.0732756853258));
#38823=CARTESIAN_POINT('',(6.28985303478256,37.2481324154382,-18.2576657286835));
#38824=CARTESIAN_POINT('',(6.32571635258722,38.5161005118285,-21.2811830997007));
#38825=CARTESIAN_POINT('',(5.33658159091048,37.53,-21.077340767532));
#38826=CARTESIAN_POINT('',(5.17788105285096,37.3520314584495,-20.9962810795385));
#38827=CARTESIAN_POINT('',(6.10937109726139,37.53,-19.3508224363324));
#38828=CARTESIAN_POINT('',(3.05468554863069,37.53,-26.1754112181662));
#38829=CARTESIAN_POINT('',(6.23934797313093,37.4321844925501,-18.8210104177224));
#38830=CARTESIAN_POINT('',(5.34401855543614,38.1059743550985,-22.4705540995224));
#38831=CARTESIAN_POINT('',(5.96554337951873,38.4299914950389,-21.8750877438693));
#38832=CARTESIAN_POINT('Origin',(6.28291460223091,37.03,-17.6727094939652));
#38833=CARTESIAN_POINT('',(6.28985303478256,64.7518675845618,-18.2576657286835));
#38834=CARTESIAN_POINT('',(6.28985303478256,37.03,-18.2576657286835));
#38835=CARTESIAN_POINT('',(6.28368335893611,64.97,-17.7375208219333));
#38836=CARTESIAN_POINT('',(6.38480703384186,61.39471468288,-26.2629224416023));
#38837=CARTESIAN_POINT('',(6.28291460223091,64.97,-17.6727094939652));
#38838=CARTESIAN_POINT('',(6.28985303478256,64.97,-18.2576657286835));
#38839=CARTESIAN_POINT('',(6.28291460223091,37.03,-17.6727094939652));
#38840=CARTESIAN_POINT('Origin',(6.28985303478256,37.03,-18.2576657286835));
#38841=CARTESIAN_POINT('',(6.23934797313093,64.5678155074499,-18.8210104177224));
#38842=CARTESIAN_POINT('',(6.23934797313093,37.03,-18.8210104177224));
#38843=CARTESIAN_POINT('',(5.59848523123102,62.2323640708404,-25.9693359567049));
#38844=CARTESIAN_POINT('Origin',(4.03106188917902,37.28,-27.8550737023638));
#38845=CARTESIAN_POINT('',(9.15969119168187,37.4321844925501,-20.5070713610788));
#38846=CARTESIAN_POINT('',(8.76584896227005,37.53,-20.8845406467914));
#38847=CARTESIAN_POINT('',(5.93055826671154,38.2341789260846,-23.6019616690071));
#38848=CARTESIAN_POINT('',(7.65703498052716,37.53,-22.4170551566691));
#38849=CARTESIAN_POINT('',(3.82851749026359,37.53,-27.7085275783346));
#38850=CARTESIAN_POINT('',(7.51456472435969,37.6995434345929,-22.3247340097329));
#38851=CARTESIAN_POINT('',(9.62230947265072,37.2481324154382,-20.1816603501494));
#38852=CARTESIAN_POINT('',(6.45071205345202,38.7735167359811,-21.9629644581006));
#38853=CARTESIAN_POINT('',(6.11180584490169,38.6447816854218,-22.6509889118845));
#38854=CARTESIAN_POINT('Origin',(7.65703498052716,37.03,-22.4170551566691));
#38855=CARTESIAN_POINT('',(8.76584896227005,64.47,-20.8845406467914));
#38856=CARTESIAN_POINT('',(8.76584896227005,37.03,-20.8845406467914));
#38857=CARTESIAN_POINT('',(7.65703498052716,64.47,-22.4170551566691));
#38858=CARTESIAN_POINT('',(3.82851749026359,64.47,-27.7085275783346));
#38859=CARTESIAN_POINT('',(7.65703498052716,37.03,-22.4170551566691));
#38860=CARTESIAN_POINT('Origin',(8.76584896227005,37.03,-20.8845406467914));
#38861=CARTESIAN_POINT('',(9.15969119168187,64.5678155074499,-20.5070713610788));
#38862=CARTESIAN_POINT('',(9.15969119168187,37.03,-20.5070713610788));
#38863=CARTESIAN_POINT('',(4.17846180539155,63.3306666093445,-25.2812193777137));
#38864=CARTESIAN_POINT('Origin',(6.06346514907441,37.28,-30.5598940702379));
#38865=CARTESIAN_POINT('',(14.1789895822776,37.4321844925501,-26.7606520268691));
#38866=CARTESIAN_POINT('',(13.6491775636676,37.53,-26.8906289027386));
#38867=CARTESIAN_POINT('',(9.83503328309243,38.2341789260845,-27.8263391929761));
#38868=CARTESIAN_POINT('',(11.922659232468,37.53,-27.6634184090895));
#38869=CARTESIAN_POINT('',(5.96132961623402,37.53,-30.3317092045448));
#38870=CARTESIAN_POINT('',(11.8454369448115,37.6995434345929,-27.5122308224524));
#38871=CARTESIAN_POINT('',(14.7423342713165,37.2481324154382,-26.7101469652175));
#38872=CARTESIAN_POINT('',(11.1049982817376,38.773516735981,-26.6670028649695));
#38873=CARTESIAN_POINT('',(10.4674846687408,38.6447816854218,-27.093396416096));
#38874=CARTESIAN_POINT('Origin',(11.922659232468,37.03,-27.6634184090895));
#38875=CARTESIAN_POINT('',(13.6491775636676,64.47,-26.8906289027386));
#38876=CARTESIAN_POINT('',(13.6491775636676,37.03,-26.8906289027386));
#38877=CARTESIAN_POINT('',(11.922659232468,64.47,-27.6634184090895));
#38878=CARTESIAN_POINT('',(5.96132961623402,64.47,-30.3317092045448));
#38879=CARTESIAN_POINT('',(11.922659232468,37.03,-27.6634184090895));
#38880=CARTESIAN_POINT('Origin',(13.6491775636676,37.03,-26.8906289027386));
#38881=CARTESIAN_POINT('',(14.1789895822776,64.5678155074499,-26.7606520268691));
#38882=CARTESIAN_POINT('',(14.1789895822776,37.03,-26.7606520268691));
#38883=CARTESIAN_POINT('',(7.47804438335529,63.3306666093445,-28.4045707975568));
#38884=CARTESIAN_POINT('Origin',(6.47116781894107,37.28,-33.9185388514382));
#38885=CARTESIAN_POINT('',(15.3990391648128,37.4321844925501,-34.6860609433565));
#38886=CARTESIAN_POINT('',(14.8752200595314,37.53,-34.533718210459));
#38887=CARTESIAN_POINT('',(11.1042190737355,38.2341789260845,-33.4369949520996));
#38888=CARTESIAN_POINT('',(12.9936165714376,37.53,-34.3397143891372));
#38889=CARTESIAN_POINT('',(6.49680828571882,37.53,-33.6698571945686));
#38890=CARTESIAN_POINT('',(13.0023339019072,37.6995434345929,-34.1701709545443));
#38891=CARTESIAN_POINT('',(15.9121625074333,37.2481324154382,-34.9239946214659));
#38892=CARTESIAN_POINT('',(12.7837091884825,38.773516735981,-33.0679627398383));
#38893=CARTESIAN_POINT('',(12.0184094288058,38.6447816854218,-33.1184735806253));
#38894=CARTESIAN_POINT('Origin',(12.9936165714376,37.03,-34.3397143891372));
#38895=CARTESIAN_POINT('',(14.8752200595314,64.47,-34.533718210459));
#38896=CARTESIAN_POINT('',(14.8752200595314,37.03,-34.533718210459));
#38897=CARTESIAN_POINT('',(12.9936165714376,64.47,-34.3397143891372));
#38898=CARTESIAN_POINT('',(6.49680828571882,64.47,-33.6698571945686));
#38899=CARTESIAN_POINT('',(12.9936165714376,37.03,-34.3397143891372));
#38900=CARTESIAN_POINT('Origin',(14.8752200595314,37.03,-34.533718210459));
#38901=CARTESIAN_POINT('',(15.3990391648128,64.5678155074499,-34.6860609433565));
#38902=CARTESIAN_POINT('',(15.3990391648128,37.03,-34.6860609433565));
#38903=CARTESIAN_POINT('',(8.77389100783484,63.3306666093446,-32.759263761069));
#38904=CARTESIAN_POINT('Origin',(5.1449262976362,37.28,-37.031061889179));
#38905=CARTESIAN_POINT('',(12.4929286389212,37.4321844925501,-42.1596911916819));
#38906=CARTESIAN_POINT('',(12.1154593532086,37.53,-41.76584896227));
#38907=CARTESIAN_POINT('',(9.39803833099293,38.2341789260846,-38.9305582667115));
#38908=CARTESIAN_POINT('',(10.5829448433309,37.53,-40.6570349805272));
#38909=CARTESIAN_POINT('',(5.29147242166543,37.53,-36.8285174902636));
#38910=CARTESIAN_POINT('',(10.6752659902672,37.6995434345929,-40.5145647243597));
#38911=CARTESIAN_POINT('',(12.8183396498506,37.2481324154382,-42.6223094726507));
#38912=CARTESIAN_POINT('',(11.0370355418994,38.7735167359811,-39.450712053452));
#38913=CARTESIAN_POINT('',(10.3490110881154,38.6447816854217,-39.1118058449017));
#38914=CARTESIAN_POINT('Origin',(10.5829448433309,37.03,-40.6570349805272));
#38915=CARTESIAN_POINT('',(12.1154593532086,64.47,-41.76584896227));
#38916=CARTESIAN_POINT('',(12.1154593532086,37.03,-41.76584896227));
#38917=CARTESIAN_POINT('',(10.5829448433309,64.47,-40.6570349805272));
#38918=CARTESIAN_POINT('',(5.29147242166543,64.47,-36.8285174902636));
#38919=CARTESIAN_POINT('',(10.5829448433309,37.03,-40.6570349805272));
#38920=CARTESIAN_POINT('Origin',(12.1154593532086,37.03,-41.76584896227));
#38921=CARTESIAN_POINT('',(12.4929286389212,64.5678155074499,-42.1596911916819));
#38922=CARTESIAN_POINT('',(12.4929286389212,37.03,-42.1596911916819));
#38923=CARTESIAN_POINT('',(7.71878062228625,63.3306666093444,-37.1784618053914));
#38924=CARTESIAN_POINT('Origin',(2.44010592976207,37.28,-39.0634651490744));
#38925=CARTESIAN_POINT('',(6.23934797313093,37.4321844925501,-47.1789895822776));
#38926=CARTESIAN_POINT('',(6.10937109726138,37.53,-46.6491775636676));
#38927=CARTESIAN_POINT('',(5.17366080702395,38.2341789260845,-42.8350332830924));
#38928=CARTESIAN_POINT('',(5.33658159091047,37.53,-44.922659232468));
#38929=CARTESIAN_POINT('',(2.66829079545524,37.53,-38.961329616234));
#38930=CARTESIAN_POINT('',(5.48776917754755,37.6995434345929,-44.8454369448115));
#38931=CARTESIAN_POINT('',(6.28985303478254,37.2481324154382,-47.7423342713165));
#38932=CARTESIAN_POINT('',(6.33299713503051,38.773516735981,-44.1049982817375));
#38933=CARTESIAN_POINT('',(5.90660358390404,38.6447816854218,-43.4674846687409));
#38934=CARTESIAN_POINT('Origin',(5.33658159091047,37.03,-44.922659232468));
#38935=CARTESIAN_POINT('',(6.10937109726138,64.47,-46.6491775636676));
#38936=CARTESIAN_POINT('',(6.10937109726138,37.03,-46.6491775636676));
#38937=CARTESIAN_POINT('',(5.33658159091047,64.47,-44.922659232468));
#38938=CARTESIAN_POINT('',(2.66829079545524,64.47,-38.961329616234));
#38939=CARTESIAN_POINT('',(5.33658159091047,37.03,-44.922659232468));
#38940=CARTESIAN_POINT('Origin',(6.10937109726138,37.03,-46.6491775636676));
#38941=CARTESIAN_POINT('',(6.23934797313093,64.5678155074499,-47.1789895822776));
#38942=CARTESIAN_POINT('',(6.23934797313093,37.03,-47.1789895822776));
#38943=CARTESIAN_POINT('',(4.5954292024432,63.3306666093445,-40.4780443833553));
#38944=CARTESIAN_POINT('Origin',(-0.918538851438202,37.28,-39.4711678189411));
#38945=CARTESIAN_POINT('',(-1.68606094335648,37.4321844925501,-48.3990391648128));
#38946=CARTESIAN_POINT('',(-1.53371821045903,37.53,-47.8752200595314));
#38947=CARTESIAN_POINT('',(-0.436994952099579,38.2341789260845,-44.1042190737355));
#38948=CARTESIAN_POINT('',(-1.33971438913717,37.53,-45.9936165714376));
#38949=CARTESIAN_POINT('',(-0.669857194568582,37.53,-39.4968082857188));
#38950=CARTESIAN_POINT('',(-1.17017095454431,37.6995434345929,-46.0023339019072));
#38951=CARTESIAN_POINT('',(-1.92399462146589,37.2481324154382,-48.9121625074333));
#38952=CARTESIAN_POINT('',(-0.0679627398382643,38.773516735981,-45.7837091884825));
#38953=CARTESIAN_POINT('',(-0.118473580625308,38.6447816854218,-45.0184094288058));
#38954=CARTESIAN_POINT('Origin',(-1.33971438913717,37.03,-45.9936165714376));
#38955=CARTESIAN_POINT('',(-1.53371821045903,64.47,-47.8752200595314));
#38956=CARTESIAN_POINT('',(-1.53371821045903,37.03,-47.8752200595314));
#38957=CARTESIAN_POINT('',(-1.33971438913717,64.47,-45.9936165714376));
#38958=CARTESIAN_POINT('',(-0.669857194568582,64.47,-39.4968082857188));
#38959=CARTESIAN_POINT('',(-1.33971438913717,37.03,-45.9936165714376));
#38960=CARTESIAN_POINT('Origin',(-1.53371821045903,37.03,-47.8752200595314));
#38961=CARTESIAN_POINT('',(-1.68606094335648,64.5678155074499,-48.3990391648128));
#38962=CARTESIAN_POINT('',(-1.68606094335648,37.03,-48.3990391648128));
#38963=CARTESIAN_POINT('',(0.240736238931031,63.3306666093445,-41.7738910078348));
#38964=CARTESIAN_POINT('Origin',(-4.03106188917902,37.28,-38.1449262976362));
#38965=CARTESIAN_POINT('',(-9.15969119168187,37.4321844925501,-45.4929286389212));
#38966=CARTESIAN_POINT('',(-8.76584896227005,37.53,-45.1154593532086));
#38967=CARTESIAN_POINT('',(-5.93055826671154,38.2341789260845,-42.3980383309929));
#38968=CARTESIAN_POINT('',(-7.65703498052716,37.53,-43.5829448433309));
#38969=CARTESIAN_POINT('',(-3.82851749026359,37.53,-38.2914724216654));
#38970=CARTESIAN_POINT('',(-7.51456472435969,37.6995434345929,-43.6752659902671));
#38971=CARTESIAN_POINT('',(-9.62230947265071,37.2481324154382,-45.8183396498506));
#38972=CARTESIAN_POINT('',(-6.45071205345204,38.7735167359811,-44.0370355418994));
#38973=CARTESIAN_POINT('',(-6.11180584490168,38.6447816854217,-43.3490110881154));
#38974=CARTESIAN_POINT('Origin',(-7.65703498052716,37.03,-43.5829448433309));
#38975=CARTESIAN_POINT('',(-8.76584896227005,64.47,-45.1154593532086));
#38976=CARTESIAN_POINT('',(-8.76584896227005,37.03,-45.1154593532086));
#38977=CARTESIAN_POINT('',(-7.65703498052716,64.47,-43.5829448433309));
#38978=CARTESIAN_POINT('',(-3.82851749026359,64.47,-38.2914724216654));
#38979=CARTESIAN_POINT('',(-7.65703498052716,37.03,-43.5829448433309));
#38980=CARTESIAN_POINT('Origin',(-8.76584896227005,37.03,-45.1154593532086));
#38981=CARTESIAN_POINT('',(-9.15969119168187,64.5678155074499,-45.4929286389212));
#38982=CARTESIAN_POINT('',(-9.15969119168187,37.03,-45.4929286389212));
#38983=CARTESIAN_POINT('',(-4.17846180539157,63.3306666093445,-40.7187806222863));
#38984=CARTESIAN_POINT('Origin',(-6.06346514907441,37.28,-35.4401059297621));
#38985=CARTESIAN_POINT('',(-14.1789895822776,37.4321844925501,-39.2393479731309));
#38986=CARTESIAN_POINT('',(-13.6491775636676,37.53,-39.1093710972614));
#38987=CARTESIAN_POINT('',(-9.83503328309245,38.2341789260846,-38.173660807024));
#38988=CARTESIAN_POINT('',(-11.922659232468,37.53,-38.3365815909105));
#38989=CARTESIAN_POINT('',(-5.96132961623402,37.53,-35.6682907954552));
#38990=CARTESIAN_POINT('',(-11.8454369448115,37.6995434345929,-38.4877691775476));
#38991=CARTESIAN_POINT('',(-14.7423342713165,37.2481324154382,-39.2898530347826));
#38992=CARTESIAN_POINT('',(-11.1049982817375,38.773516735981,-39.3329971350305));
#38993=CARTESIAN_POINT('',(-10.4674846687408,38.6447816854218,-38.906603583904));
#38994=CARTESIAN_POINT('Origin',(-11.922659232468,37.03,-38.3365815909105));
#38995=CARTESIAN_POINT('',(-13.6491775636676,64.47,-39.1093710972614));
#38996=CARTESIAN_POINT('',(-13.6491775636676,37.03,-39.1093710972614));
#38997=CARTESIAN_POINT('',(-11.922659232468,64.47,-38.3365815909105));
#38998=CARTESIAN_POINT('',(-5.96132961623402,64.47,-35.6682907954552));
#38999=CARTESIAN_POINT('',(-11.922659232468,37.03,-38.3365815909105));
#39000=CARTESIAN_POINT('Origin',(-13.6491775636676,37.03,-39.1093710972614));
#39001=CARTESIAN_POINT('',(-14.1789895822776,64.5678155074499,-39.2393479731309));
#39002=CARTESIAN_POINT('',(-14.1789895822776,37.03,-39.2393479731309));
#39003=CARTESIAN_POINT('',(-7.47804438335517,63.3306666093444,-37.5954292024432));
#39004=CARTESIAN_POINT('Origin',(-6.47116781894107,37.28,-32.0814611485618));
#39005=CARTESIAN_POINT('',(-15.3990391648128,37.4321844925501,-31.3139390566435));
#39006=CARTESIAN_POINT('',(-14.8752200595314,37.53,-31.466281789541));
#39007=CARTESIAN_POINT('',(-11.1042190737355,38.2341789260846,-32.5630050479005));
#39008=CARTESIAN_POINT('',(-12.9936165714376,37.53,-31.6602856108628));
#39009=CARTESIAN_POINT('',(-6.49680828571882,37.53,-32.3301428054314));
#39010=CARTESIAN_POINT('',(-13.0023339019072,37.6995434345929,-31.8298290454557));
#39011=CARTESIAN_POINT('',(-15.9121625074333,37.2481324154382,-31.0760053785341));
#39012=CARTESIAN_POINT('',(-12.7837091884825,38.773516735981,-32.9320372601617));
#39013=CARTESIAN_POINT('',(-12.0184094288057,38.6447816854217,-32.8815264193746));
#39014=CARTESIAN_POINT('Origin',(-12.9936165714376,37.03,-31.6602856108628));
#39015=CARTESIAN_POINT('',(-14.8752200595314,64.47,-31.466281789541));
#39016=CARTESIAN_POINT('',(-14.8752200595314,37.03,-31.466281789541));
#39017=CARTESIAN_POINT('',(-12.9936165714376,64.47,-31.6602856108628));
#39018=CARTESIAN_POINT('',(-6.49680828571882,64.47,-32.3301428054314));
#39019=CARTESIAN_POINT('',(-12.9936165714376,37.03,-31.6602856108628));
#39020=CARTESIAN_POINT('Origin',(-14.8752200595314,37.03,-31.466281789541));
#39021=CARTESIAN_POINT('',(-15.3990391648128,64.5678155074499,-31.3139390566435));
#39022=CARTESIAN_POINT('',(-15.3990391648128,37.03,-31.3139390566435));
#39023=CARTESIAN_POINT('',(-8.77389100783466,63.3306666093444,-33.2407362389312));
#39024=CARTESIAN_POINT('Origin',(-5.14492629763621,37.28,-28.968938110821));
#39025=CARTESIAN_POINT('',(-12.4929286389212,37.4321844925501,-23.8403088083181));
#39026=CARTESIAN_POINT('',(-12.1154593532086,37.53,-24.23415103773));
#39027=CARTESIAN_POINT('',(-9.39803833099287,38.2341789260845,-27.0694417332885));
#39028=CARTESIAN_POINT('',(-10.5829448433309,37.53,-25.3429650194728));
#39029=CARTESIAN_POINT('',(-5.29147242166544,37.53,-29.1714825097364));
#39030=CARTESIAN_POINT('',(-10.6752659902672,37.6995434345929,-25.4854352756403));
#39031=CARTESIAN_POINT('',(-12.8183396498506,37.2481324154382,-23.3776905273493));
#39032=CARTESIAN_POINT('',(-11.0370355418993,38.773516735981,-26.549287946548));
#39033=CARTESIAN_POINT('',(-10.3490110881154,38.6447816854218,-26.8881941550983));
#39034=CARTESIAN_POINT('Origin',(-10.5829448433309,37.03,-25.3429650194728));
#39035=CARTESIAN_POINT('',(-12.1154593532086,64.47,-24.23415103773));
#39036=CARTESIAN_POINT('',(-12.1154593532086,37.03,-24.23415103773));
#39037=CARTESIAN_POINT('',(-10.5829448433309,64.47,-25.3429650194728));
#39038=CARTESIAN_POINT('',(-5.29147242166544,64.47,-29.1714825097364));
#39039=CARTESIAN_POINT('',(-10.5829448433309,37.03,-25.3429650194728));
#39040=CARTESIAN_POINT('Origin',(-12.1154593532086,37.03,-24.23415103773));
#39041=CARTESIAN_POINT('',(-12.4929286389212,64.5678155074499,-23.8403088083181));
#39042=CARTESIAN_POINT('',(-12.4929286389212,37.03,-23.8403088083181));
#39043=CARTESIAN_POINT('',(-7.7187806222863,63.3306666093445,-28.8215381946084));
#39044=CARTESIAN_POINT('Origin',(-2.44010592976206,37.28,-26.9365348509256));
#39045=CARTESIAN_POINT('',(-6.23934797313094,37.4321844925501,-18.8210104177224));
#39046=CARTESIAN_POINT('',(-6.10937109726139,37.53,-19.3508224363324));
#39047=CARTESIAN_POINT('',(-5.17366080702394,38.2341789260845,-23.1649667169076));
#39048=CARTESIAN_POINT('',(-5.33658159091048,37.53,-21.077340767532));
#39049=CARTESIAN_POINT('',(-2.66829079545523,37.53,-27.038670383766));
#39050=CARTESIAN_POINT('',(-5.48776917754756,37.6995434345929,-21.1545630551885));
#39051=CARTESIAN_POINT('',(-6.28985303478256,37.2481324154382,-18.2576657286835));
#39052=CARTESIAN_POINT('',(-6.33299713503051,38.773516735981,-21.8950017182625));
#39053=CARTESIAN_POINT('',(-5.90660358390399,38.6447816854218,-22.5325153312592));
#39054=CARTESIAN_POINT('Origin',(-5.33658159091048,37.03,-21.077340767532));
#39055=CARTESIAN_POINT('',(-6.10937109726139,64.47,-19.3508224363324));
#39056=CARTESIAN_POINT('',(-6.10937109726139,37.03,-19.3508224363324));
#39057=CARTESIAN_POINT('',(-5.33658159091048,64.47,-21.077340767532));
#39058=CARTESIAN_POINT('',(-2.66829079545523,64.47,-27.038670383766));
#39059=CARTESIAN_POINT('',(-5.33658159091048,37.03,-21.077340767532));
#39060=CARTESIAN_POINT('Origin',(-6.10937109726139,37.03,-19.3508224363324));
#39061=CARTESIAN_POINT('',(-6.23934797313094,64.5678155074499,-18.8210104177224));
#39062=CARTESIAN_POINT('',(-6.23934797313094,37.03,-18.8210104177224));
#39063=CARTESIAN_POINT('',(-4.59542920244319,63.3306666093445,-25.5219556166447));
#39064=CARTESIAN_POINT('Origin',(0.918538851438207,37.28,-26.5288321810589));
#39065=CARTESIAN_POINT('',(1.68606094335648,37.4321844925501,-17.6009608351872));
#39066=CARTESIAN_POINT('',(1.53371821045903,37.53,-18.1247799404686));
#39067=CARTESIAN_POINT('',(0.43699495209958,38.2341789260845,-21.8957809262645));
#39068=CARTESIAN_POINT('',(1.33971438913717,37.53,-20.0063834285624));
#39069=CARTESIAN_POINT('',(0.669857194568587,37.53,-26.5031917142812));
#39070=CARTESIAN_POINT('',(1.17017095454432,37.6995434345929,-19.9976660980928));
#39071=CARTESIAN_POINT('',(1.92399462146589,37.2481324154382,-17.0878374925667));
#39072=CARTESIAN_POINT('',(0.0679627398382635,38.773516735981,-20.2162908115175));
#39073=CARTESIAN_POINT('',(0.118473580625342,38.6447816854218,-20.9815905711943));
#39074=CARTESIAN_POINT('Origin',(1.33971438913717,37.03,-20.0063834285624));
#39075=CARTESIAN_POINT('',(1.53371821045903,64.47,-18.1247799404686));
#39076=CARTESIAN_POINT('',(1.53371821045903,37.03,-18.1247799404686));
#39077=CARTESIAN_POINT('',(1.33971438913717,64.47,-20.0063834285624));
#39078=CARTESIAN_POINT('',(0.669857194568587,64.47,-26.5031917142812));
#39079=CARTESIAN_POINT('',(1.33971438913717,37.03,-20.0063834285624));
#39080=CARTESIAN_POINT('Origin',(1.53371821045903,37.03,-18.1247799404686));
#39081=CARTESIAN_POINT('',(1.68606094335648,64.5678155074499,-17.6009608351872));
#39082=CARTESIAN_POINT('',(1.68606094335648,37.03,-17.6009608351872));
#39083=CARTESIAN_POINT('',(-0.240736238931032,63.3306666093445,-24.2261089921652));
#39084=CARTESIAN_POINT('Origin',(2.82650068293752,64.72,-26.0732756853258));
#39085=CARTESIAN_POINT('',(6.10937109726139,64.47,-19.3508224363324));
#39086=CARTESIAN_POINT('',(4.76578695085538,63.4588711803305,-24.8275429992595));
#39087=CARTESIAN_POINT('',(5.33658159091048,64.47,-21.077340767532));
#39088=CARTESIAN_POINT('',(3.05468554863069,64.47,-26.1754112181662));
#39089=CARTESIAN_POINT('',(4.8907147633328,64.97,-20.8496047663061));
#39090=CARTESIAN_POINT('',(11.3984181516531,57.6721893244721,-24.173553208203));
#39091=CARTESIAN_POINT('',(2.59831581724435,64.97,-25.9711401524854));
#39092=CARTESIAN_POINT('Origin',(2.22044604925031E-15,64.97,-33.));
#39093=CARTESIAN_POINT('',(6.53125,64.97,-21.6875431630658));
#39094=CARTESIAN_POINT('',(6.53125,64.97,-21.6875431630658));
#39095=CARTESIAN_POINT('',(8.07719355673392,64.97,-22.6893191554432));
#39096=CARTESIAN_POINT('',(7.65703498052716,64.97,-22.4170551566691));
#39097=CARTESIAN_POINT('',(10.0758530134688,64.97,-19.9269309927904));
#39098=CARTESIAN_POINT('',(4.23360628809444,64.97,-28.001619826393));
#39099=CARTESIAN_POINT('',(10.1323656482948,64.97,-19.8951910916424));
#39100=CARTESIAN_POINT('',(10.1323656482948,64.97,-19.8951910916424));
#39101=CARTESIAN_POINT('',(10.6822399290158,64.97,-19.6444956527339));
#39102=CARTESIAN_POINT('',(10.6822399290158,64.97,-19.6444956527339));
#39103=CARTESIAN_POINT('',(11.2673077173324,64.97,-19.428591225812));
#39104=CARTESIAN_POINT('',(11.2673077173324,64.97,-19.428591225812));
#39105=CARTESIAN_POINT('',(11.8841806942968,64.97,-19.2474024814435));
#39106=CARTESIAN_POINT('',(11.8841806942968,64.97,-19.2474024814435));
#39107=CARTESIAN_POINT('',(12.5300905656334,64.97,-19.1013106159343));
#39108=CARTESIAN_POINT('',(12.5300905656334,64.97,-19.1013106159343));
#39109=CARTESIAN_POINT('',(13.2026107084364,64.97,-18.990946838509));
#39110=CARTESIAN_POINT('',(13.2026107084364,64.97,-18.990946838509));
#39111=CARTESIAN_POINT('',(13.4086793188509,64.97,-19.1880552084719));
#39112=CARTESIAN_POINT('',(13.4086793188509,64.97,-19.1880552084719));
#39113=CARTESIAN_POINT('',(13.611805537841,64.97,-19.388194462159));
#39114=CARTESIAN_POINT('',(13.611805537841,64.97,-19.388194462159));
#39115=CARTESIAN_POINT('',(13.8119447915281,64.97,-19.5913206811491));
#39116=CARTESIAN_POINT('',(13.8119447915281,64.97,-19.5913206811491));
#39117=CARTESIAN_POINT('',(14.009053161491,64.97,-19.7973892915637));
#39118=CARTESIAN_POINT('',(14.009053161491,64.97,-19.7973892915637));
#39119=CARTESIAN_POINT('',(13.8986893840657,64.97,-20.4699094343666));
#39120=CARTESIAN_POINT('',(13.8986893840657,64.97,-20.4699094343666));
#39121=CARTESIAN_POINT('',(13.7525975185565,64.97,-21.1158193057032));
#39122=CARTESIAN_POINT('',(13.7525975185565,64.97,-21.1158193057032));
#39123=CARTESIAN_POINT('',(13.571408774188,64.97,-21.7326922826676));
#39124=CARTESIAN_POINT('',(13.571408774188,64.97,-21.7326922826676));
#39125=CARTESIAN_POINT('',(13.3555043472661,64.97,-22.3177600709842));
#39126=CARTESIAN_POINT('',(13.3555043472661,64.97,-22.3177600709842));
#39127=CARTESIAN_POINT('',(13.1048089083576,64.97,-22.8676343517052));
#39128=CARTESIAN_POINT('',(10.3106808445568,64.97,-24.9228064432661));
#39129=CARTESIAN_POINT('',(5.76463742854583,64.97,-28.2119867210341));
#39130=CARTESIAN_POINT('',(11.3124568369342,64.97,-26.46875));
#39131=CARTESIAN_POINT('',(11.3124568369342,64.97,-26.46875));
#39132=CARTESIAN_POINT('',(12.1503952336939,64.97,-28.1092852366672));
#39133=CARTESIAN_POINT('',(11.922659232468,64.97,-27.6634184090895));
#39134=CARTESIAN_POINT('',(15.2624791780667,64.97,-26.7163166410639));
#39135=CARTESIAN_POINT('',(6.1656006819148,64.97,-30.7880789359311));
#39136=CARTESIAN_POINT('',(15.3272905060348,64.97,-26.7170853977691));
#39137=CARTESIAN_POINT('',(15.3272905060348,64.97,-26.7170853977691));
#39138=CARTESIAN_POINT('',(15.9288433214812,64.97,-26.774913919422));
#39139=CARTESIAN_POINT('',(15.9288433214812,64.97,-26.774913919422));
#39140=CARTESIAN_POINT('',(16.5434791025604,64.97,-26.8804690950764));
#39141=CARTESIAN_POINT('',(16.5434791025604,64.97,-26.8804690950764));
#39142=CARTESIAN_POINT('',(17.1683011437039,64.97,-27.0319915280556));
#39143=CARTESIAN_POINT('',(17.1683011437039,64.97,-27.0319915280556));
#39144=CARTESIAN_POINT('',(17.8007214335911,64.97,-27.2284271969067));
#39145=CARTESIAN_POINT('',(17.8007214335911,64.97,-27.2284271969067));
#39146=CARTESIAN_POINT('',(18.4383228505279,64.97,-27.4691094334002));
#39147=CARTESIAN_POINT('',(18.4383228505279,64.97,-27.4691094334002));
#39148=CARTESIAN_POINT('',(18.518229317088,64.97,-27.742844594294));
#39149=CARTESIAN_POINT('',(18.518229317088,64.97,-27.742844594294));
#39150=CARTESIAN_POINT('',(18.5940721560646,64.97,-28.0177333817765));
#39151=CARTESIAN_POINT('',(18.5940721560646,64.97,-28.0177333817765));
#39152=CARTESIAN_POINT('',(18.6658347245569,64.97,-28.2937154744402));
#39153=CARTESIAN_POINT('',(18.6658347245569,64.97,-28.2937154744402));
#39154=CARTESIAN_POINT('',(18.7335012750361,64.97,-28.5707303109632));
#39155=CARTESIAN_POINT('',(18.7335012750361,64.97,-28.5707303109632));
#39156=CARTESIAN_POINT('',(18.3016633687267,64.97,-29.0979679504746));
#39157=CARTESIAN_POINT('',(18.3016633687267,64.97,-29.0979679504746));
#39158=CARTESIAN_POINT('',(17.8521891662412,64.97,-29.5842963748526));
#39159=CARTESIAN_POINT('',(17.8521891662412,64.97,-29.5842963748526));
#39160=CARTESIAN_POINT('',(17.3868386222561,64.97,-30.0279296716277));
#39161=CARTESIAN_POINT('',(17.3868386222561,64.97,-30.0279296716277));
#39162=CARTESIAN_POINT('',(16.9073260095938,64.97,-30.4266610257849));
#39163=CARTESIAN_POINT('',(16.9073260095938,64.97,-30.4266610257849));
#39164=CARTESIAN_POINT('',(16.4152802505257,64.97,-30.7775184023227));
#39165=CARTESIAN_POINT('',(12.9679083200667,64.97,-31.1602856108628));
#39166=CARTESIAN_POINT('',(7.38632909621023,64.97,-31.7357775810312));
#39167=CARTESIAN_POINT('',(13.0625,64.97,-33.));
#39168=CARTESIAN_POINT('',(13.0625,64.97,-33.));
#39169=CARTESIAN_POINT('',(12.9679083200667,64.97,-34.8397143891372));
#39170=CARTESIAN_POINT('',(12.9936165714376,64.97,-34.3397143891372));
#39171=CARTESIAN_POINT('',(16.3595363724049,64.97,-35.1894101708572));
#39172=CARTESIAN_POINT('',(6.44552735216333,64.97,-34.1672205083078));
#39173=CARTESIAN_POINT('',(16.4152802505257,64.97,-35.2224815976773));
#39174=CARTESIAN_POINT('',(16.4152802505257,64.97,-35.2224815976773));
#39175=CARTESIAN_POINT('',(16.9073260095938,64.97,-35.5733389742151));
#39176=CARTESIAN_POINT('',(16.9073260095938,64.97,-35.5733389742151));
#39177=CARTESIAN_POINT('',(17.3868386222561,64.97,-35.9720703283723));
#39178=CARTESIAN_POINT('',(17.3868386222561,64.97,-35.9720703283723));
#39179=CARTESIAN_POINT('',(17.8521891662412,64.97,-36.4157036251474));
#39180=CARTESIAN_POINT('',(17.8521891662412,64.97,-36.4157036251474));
#39181=CARTESIAN_POINT('',(18.3016633687267,64.97,-36.9020320495254));
#39182=CARTESIAN_POINT('',(18.3016633687267,64.97,-36.9020320495254));
#39183=CARTESIAN_POINT('',(18.7335012750361,64.97,-37.4292696890368));
#39184=CARTESIAN_POINT('',(18.7335012750361,64.97,-37.4292696890368));
#39185=CARTESIAN_POINT('',(18.6658347245569,64.97,-37.7062845255599));
#39186=CARTESIAN_POINT('',(18.6658347245569,64.97,-37.7062845255599));
#39187=CARTESIAN_POINT('',(18.5940721560646,64.97,-37.9822666182235));
#39188=CARTESIAN_POINT('',(18.5940721560646,64.97,-37.9822666182235));
#39189=CARTESIAN_POINT('',(18.518229317088,64.97,-38.257155405706));
#39190=CARTESIAN_POINT('',(18.518229317088,64.97,-38.257155405706));
#39191=CARTESIAN_POINT('',(18.4383228505279,64.97,-38.5308905665998));
#39192=CARTESIAN_POINT('',(18.4383228505279,64.97,-38.5308905665998));
#39193=CARTESIAN_POINT('',(17.8007214335911,64.97,-38.7715728030933));
#39194=CARTESIAN_POINT('',(17.8007214335911,64.97,-38.7715728030933));
#39195=CARTESIAN_POINT('',(17.1683011437039,64.97,-38.9680084719444));
#39196=CARTESIAN_POINT('',(17.1683011437039,64.97,-38.9680084719444));
#39197=CARTESIAN_POINT('',(16.5434791025604,64.97,-39.1195309049236));
#39198=CARTESIAN_POINT('',(16.5434791025604,64.97,-39.1195309049236));
#39199=CARTESIAN_POINT('',(15.9288433214812,64.97,-39.225086080578));
#39200=CARTESIAN_POINT('',(15.9288433214812,64.97,-39.225086080578));
#39201=CARTESIAN_POINT('',(15.3272905060348,64.97,-39.2829146022309));
#39202=CARTESIAN_POINT('',(12.1503952336939,64.97,-37.8907147633328));
#39203=CARTESIAN_POINT('',(7.02885984751459,64.97,-35.5983158172444));
#39204=CARTESIAN_POINT('',(11.3124568369342,64.97,-39.53125));
#39205=CARTESIAN_POINT('',(11.3124568369342,64.97,-39.53125));
#39206=CARTESIAN_POINT('',(10.3106808445568,64.97,-41.0771935567339));
#39207=CARTESIAN_POINT('',(10.5829448433309,64.97,-40.6570349805272));
#39208=CARTESIAN_POINT('',(13.0730690072096,64.97,-43.0758530134688));
#39209=CARTESIAN_POINT('',(4.99838017360697,64.97,-37.2336062880944));
#39210=CARTESIAN_POINT('',(13.1048089083576,64.97,-43.1323656482948));
#39211=CARTESIAN_POINT('',(13.1048089083576,64.97,-43.1323656482948));
#39212=CARTESIAN_POINT('',(13.3555043472661,64.97,-43.6822399290158));
#39213=CARTESIAN_POINT('',(13.3555043472661,64.97,-43.6822399290158));
#39214=CARTESIAN_POINT('',(13.571408774188,64.97,-44.2673077173324));
#39215=CARTESIAN_POINT('',(13.571408774188,64.97,-44.2673077173324));
#39216=CARTESIAN_POINT('',(13.7525975185565,64.97,-44.8841806942968));
#39217=CARTESIAN_POINT('',(13.7525975185565,64.97,-44.8841806942968));
#39218=CARTESIAN_POINT('',(13.8986893840657,64.97,-45.5300905656334));
#39219=CARTESIAN_POINT('',(13.8986893840657,64.97,-45.5300905656334));
#39220=CARTESIAN_POINT('',(14.009053161491,64.97,-46.2026107084364));
#39221=CARTESIAN_POINT('',(14.009053161491,64.97,-46.2026107084364));
#39222=CARTESIAN_POINT('',(13.8119447915281,64.97,-46.4086793188509));
#39223=CARTESIAN_POINT('',(13.8119447915281,64.97,-46.4086793188509));
#39224=CARTESIAN_POINT('',(13.611805537841,64.97,-46.6118055378411));
#39225=CARTESIAN_POINT('',(13.611805537841,64.97,-46.6118055378411));
#39226=CARTESIAN_POINT('',(13.4086793188509,64.97,-46.8119447915281));
#39227=CARTESIAN_POINT('',(13.4086793188509,64.97,-46.8119447915281));
#39228=CARTESIAN_POINT('',(13.2026107084363,64.97,-47.009053161491));
#39229=CARTESIAN_POINT('',(13.2026107084363,64.97,-47.009053161491));
#39230=CARTESIAN_POINT('',(12.5300905656334,64.97,-46.8986893840657));
#39231=CARTESIAN_POINT('',(12.5300905656334,64.97,-46.8986893840657));
#39232=CARTESIAN_POINT('',(11.8841806942968,64.97,-46.7525975185565));
#39233=CARTESIAN_POINT('',(11.8841806942968,64.97,-46.7525975185565));
#39234=CARTESIAN_POINT('',(11.2673077173324,64.97,-46.571408774188));
#39235=CARTESIAN_POINT('',(11.2673077173324,64.97,-46.571408774188));
#39236=CARTESIAN_POINT('',(10.6822399290158,64.97,-46.3555043472661));
#39237=CARTESIAN_POINT('',(10.6822399290158,64.97,-46.3555043472661));
#39238=CARTESIAN_POINT('',(10.1323656482948,64.97,-46.1048089083576));
#39239=CARTESIAN_POINT('',(8.07719355673392,64.97,-43.3106808445568));
#39240=CARTESIAN_POINT('',(4.78801327896586,64.97,-38.7646374285458));
#39241=CARTESIAN_POINT('',(6.53125,64.97,-44.3124568369342));
#39242=CARTESIAN_POINT('',(6.53125,64.97,-44.3124568369342));
#39243=CARTESIAN_POINT('',(4.89071476333279,64.97,-45.1503952336939));
#39244=CARTESIAN_POINT('',(5.33658159091047,64.97,-44.922659232468));
#39245=CARTESIAN_POINT('',(6.2836833589361,64.97,-48.2624791780667));
#39246=CARTESIAN_POINT('',(2.2119210640689,64.97,-39.1656006819148));
#39247=CARTESIAN_POINT('',(6.2829146022309,64.97,-48.3272905060348));
#39248=CARTESIAN_POINT('',(6.2829146022309,64.97,-48.3272905060348));
#39249=CARTESIAN_POINT('',(6.22508608057804,64.97,-48.9288433214812));
#39250=CARTESIAN_POINT('',(6.22508608057804,64.97,-48.9288433214812));
#39251=CARTESIAN_POINT('',(6.11953090492363,64.97,-49.5434791025604));
#39252=CARTESIAN_POINT('',(6.11953090492363,64.97,-49.5434791025604));
#39253=CARTESIAN_POINT('',(5.96800847194436,64.97,-50.1683011437039));
#39254=CARTESIAN_POINT('',(5.96800847194436,64.97,-50.1683011437039));
#39255=CARTESIAN_POINT('',(5.77157280309329,64.97,-50.8007214335911));
#39256=CARTESIAN_POINT('',(5.77157280309329,64.97,-50.8007214335911));
#39257=CARTESIAN_POINT('',(5.53089056659975,64.97,-51.4383228505279));
#39258=CARTESIAN_POINT('',(5.53089056659975,64.97,-51.4383228505279));
#39259=CARTESIAN_POINT('',(5.25715540570603,64.97,-51.518229317088));
#39260=CARTESIAN_POINT('',(5.25715540570603,64.97,-51.518229317088));
#39261=CARTESIAN_POINT('',(4.98226661822352,64.97,-51.5940721560646));
#39262=CARTESIAN_POINT('',(4.98226661822352,64.97,-51.5940721560646));
#39263=CARTESIAN_POINT('',(4.70628452555985,64.97,-51.6658347245569));
#39264=CARTESIAN_POINT('',(4.70628452555985,64.97,-51.6658347245569));
#39265=CARTESIAN_POINT('',(4.42926968903682,64.97,-51.7335012750361));
#39266=CARTESIAN_POINT('',(4.42926968903682,64.97,-51.7335012750361));
#39267=CARTESIAN_POINT('',(3.90203204952538,64.97,-51.3016633687267));
#39268=CARTESIAN_POINT('',(3.90203204952538,64.97,-51.3016633687267));
#39269=CARTESIAN_POINT('',(3.41570362514738,64.97,-50.8521891662412));
#39270=CARTESIAN_POINT('',(3.41570362514738,64.97,-50.8521891662412));
#39271=CARTESIAN_POINT('',(2.97207032837233,64.97,-50.3868386222561));
#39272=CARTESIAN_POINT('',(2.97207032837233,64.97,-50.3868386222561));
#39273=CARTESIAN_POINT('',(2.57333897421511,64.97,-49.9073260095938));
#39274=CARTESIAN_POINT('',(2.57333897421511,64.97,-49.9073260095938));
#39275=CARTESIAN_POINT('',(2.22248159767725,64.97,-49.4152802505257));
#39276=CARTESIAN_POINT('',(1.83971438913716,64.97,-45.9679083200667));
#39277=CARTESIAN_POINT('',(1.26422241896875,64.97,-40.3863290962102));
#39278=CARTESIAN_POINT('',(-2.22044604925031E-15,64.97,-46.0625));
#39279=CARTESIAN_POINT('',(-2.39954232207934E-15,64.97,-46.0625));
#39280=CARTESIAN_POINT('',(-1.83971438913717,64.97,-45.9679083200667));
#39281=CARTESIAN_POINT('',(-1.33971438913717,64.97,-45.9936165714376));
#39282=CARTESIAN_POINT('',(-2.18941017085716,64.97,-49.3595363724049));
#39283=CARTESIAN_POINT('',(-1.16722050830782,64.97,-39.4455273521633));
#39284=CARTESIAN_POINT('',(-2.22248159767726,64.97,-49.4152802505257));
#39285=CARTESIAN_POINT('',(-2.22248159767726,64.97,-49.4152802505257));
#39286=CARTESIAN_POINT('',(-2.57333897421511,64.97,-49.9073260095938));
#39287=CARTESIAN_POINT('',(-2.57333897421511,64.97,-49.9073260095938));
#39288=CARTESIAN_POINT('',(-2.97207032837233,64.97,-50.3868386222561));
#39289=CARTESIAN_POINT('',(-2.97207032837234,64.97,-50.3868386222561));
#39290=CARTESIAN_POINT('',(-3.41570362514738,64.97,-50.8521891662412));
#39291=CARTESIAN_POINT('',(-3.41570362514739,64.97,-50.8521891662412));
#39292=CARTESIAN_POINT('',(-3.90203204952539,64.97,-51.3016633687267));
#39293=CARTESIAN_POINT('',(-3.90203204952539,64.97,-51.3016633687267));
#39294=CARTESIAN_POINT('',(-4.42926968903682,64.97,-51.7335012750361));
#39295=CARTESIAN_POINT('',(-4.42926968903682,64.97,-51.7335012750361));
#39296=CARTESIAN_POINT('',(-4.70628452555985,64.97,-51.6658347245569));
#39297=CARTESIAN_POINT('',(-4.70628452555985,64.97,-51.6658347245569));
#39298=CARTESIAN_POINT('',(-4.98226661822352,64.97,-51.5940721560646));
#39299=CARTESIAN_POINT('',(-4.98226661822352,64.97,-51.5940721560646));
#39300=CARTESIAN_POINT('',(-5.25715540570604,64.97,-51.518229317088));
#39301=CARTESIAN_POINT('',(-5.25715540570604,64.97,-51.518229317088));
#39302=CARTESIAN_POINT('',(-5.53089056659976,64.97,-51.4383228505279));
#39303=CARTESIAN_POINT('',(-5.53089056659976,64.97,-51.4383228505279));
#39304=CARTESIAN_POINT('',(-5.7715728030933,64.97,-50.8007214335911));
#39305=CARTESIAN_POINT('',(-5.7715728030933,64.97,-50.8007214335911));
#39306=CARTESIAN_POINT('',(-5.96800847194436,64.97,-50.1683011437039));
#39307=CARTESIAN_POINT('',(-5.96800847194436,64.97,-50.1683011437039));
#39308=CARTESIAN_POINT('',(-6.11953090492364,64.97,-49.5434791025604));
#39309=CARTESIAN_POINT('',(-6.11953090492364,64.97,-49.5434791025604));
#39310=CARTESIAN_POINT('',(-6.22508608057804,64.97,-48.9288433214812));
#39311=CARTESIAN_POINT('',(-6.22508608057804,64.97,-48.9288433214812));
#39312=CARTESIAN_POINT('',(-6.2829146022309,64.97,-48.3272905060348));
#39313=CARTESIAN_POINT('',(-4.8907147633328,64.97,-45.1503952336939));
#39314=CARTESIAN_POINT('',(-2.59831581724436,64.97,-40.0288598475146));
#39315=CARTESIAN_POINT('',(-6.53125000000001,64.97,-44.3124568369342));
#39316=CARTESIAN_POINT('',(-6.53125000000001,64.97,-44.3124568369342));
#39317=CARTESIAN_POINT('',(-8.07719355673392,64.97,-43.3106808445568));
#39318=CARTESIAN_POINT('',(-7.65703498052716,64.97,-43.5829448433309));
#39319=CARTESIAN_POINT('',(-10.0758530134688,64.97,-46.0730690072096));
#39320=CARTESIAN_POINT('',(-4.23360628809444,64.97,-37.998380173607));
#39321=CARTESIAN_POINT('',(-10.1323656482948,64.97,-46.1048089083576));
#39322=CARTESIAN_POINT('',(-10.1323656482948,64.97,-46.1048089083576));
#39323=CARTESIAN_POINT('',(-10.6822399290158,64.97,-46.3555043472661));
#39324=CARTESIAN_POINT('',(-10.6822399290158,64.97,-46.3555043472661));
#39325=CARTESIAN_POINT('',(-11.2673077173324,64.97,-46.571408774188));
#39326=CARTESIAN_POINT('',(-11.2673077173324,64.97,-46.571408774188));
#39327=CARTESIAN_POINT('',(-11.8841806942968,64.97,-46.7525975185565));
#39328=CARTESIAN_POINT('',(-11.8841806942968,64.97,-46.7525975185565));
#39329=CARTESIAN_POINT('',(-12.5300905656334,64.97,-46.8986893840657));
#39330=CARTESIAN_POINT('',(-12.5300905656334,64.97,-46.8986893840657));
#39331=CARTESIAN_POINT('',(-13.2026107084363,64.97,-47.009053161491));
#39332=CARTESIAN_POINT('',(-13.2026107084363,64.97,-47.009053161491));
#39333=CARTESIAN_POINT('',(-13.4086793188509,64.97,-46.8119447915281));
#39334=CARTESIAN_POINT('',(-13.4086793188509,64.97,-46.8119447915281));
#39335=CARTESIAN_POINT('',(-13.611805537841,64.97,-46.611805537841));
#39336=CARTESIAN_POINT('',(-13.611805537841,64.97,-46.611805537841));
#39337=CARTESIAN_POINT('',(-13.8119447915281,64.97,-46.4086793188509));
#39338=CARTESIAN_POINT('',(-13.8119447915281,64.97,-46.4086793188509));
#39339=CARTESIAN_POINT('',(-14.009053161491,64.97,-46.2026107084363));
#39340=CARTESIAN_POINT('',(-14.009053161491,64.97,-46.2026107084363));
#39341=CARTESIAN_POINT('',(-13.8986893840657,64.97,-45.5300905656334));
#39342=CARTESIAN_POINT('',(-13.8986893840657,64.97,-45.5300905656334));
#39343=CARTESIAN_POINT('',(-13.7525975185565,64.97,-44.8841806942968));
#39344=CARTESIAN_POINT('',(-13.7525975185565,64.97,-44.8841806942968));
#39345=CARTESIAN_POINT('',(-13.571408774188,64.97,-44.2673077173324));
#39346=CARTESIAN_POINT('',(-13.571408774188,64.97,-44.2673077173324));
#39347=CARTESIAN_POINT('',(-13.3555043472661,64.97,-43.6822399290158));
#39348=CARTESIAN_POINT('',(-13.3555043472661,64.97,-43.6822399290158));
#39349=CARTESIAN_POINT('',(-13.1048089083576,64.97,-43.1323656482948));
#39350=CARTESIAN_POINT('',(-10.3106808445568,64.97,-41.0771935567339));
#39351=CARTESIAN_POINT('',(-5.76463742854584,64.97,-37.7880132789659));
#39352=CARTESIAN_POINT('',(-11.3124568369342,64.97,-39.53125));
#39353=CARTESIAN_POINT('',(-11.3124568369342,64.97,-39.53125));
#39354=CARTESIAN_POINT('',(-12.1503952336939,64.97,-37.8907147633328));
#39355=CARTESIAN_POINT('',(-11.922659232468,64.97,-38.3365815909105));
#39356=CARTESIAN_POINT('',(-15.2624791780667,64.97,-39.2836833589361));
#39357=CARTESIAN_POINT('',(-6.16560068191481,64.97,-35.2119210640689));
#39358=CARTESIAN_POINT('',(-15.3272905060348,64.97,-39.2829146022309));
#39359=CARTESIAN_POINT('',(-15.3272905060348,64.97,-39.2829146022309));
#39360=CARTESIAN_POINT('',(-15.9288433214812,64.97,-39.225086080578));
#39361=CARTESIAN_POINT('',(-15.9288433214812,64.97,-39.225086080578));
#39362=CARTESIAN_POINT('',(-16.5434791025604,64.97,-39.1195309049236));
#39363=CARTESIAN_POINT('',(-16.5434791025604,64.97,-39.1195309049236));
#39364=CARTESIAN_POINT('',(-17.1683011437039,64.97,-38.9680084719444));
#39365=CARTESIAN_POINT('',(-17.1683011437039,64.97,-38.9680084719444));
#39366=CARTESIAN_POINT('',(-17.8007214335911,64.97,-38.7715728030933));
#39367=CARTESIAN_POINT('',(-17.8007214335911,64.97,-38.7715728030933));
#39368=CARTESIAN_POINT('',(-18.4383228505279,64.97,-38.5308905665998));
#39369=CARTESIAN_POINT('',(-18.4383228505279,64.97,-38.5308905665998));
#39370=CARTESIAN_POINT('',(-18.518229317088,64.97,-38.257155405706));
#39371=CARTESIAN_POINT('',(-18.518229317088,64.97,-38.257155405706));
#39372=CARTESIAN_POINT('',(-18.5940721560646,64.97,-37.9822666182235));
#39373=CARTESIAN_POINT('',(-18.5940721560646,64.97,-37.9822666182235));
#39374=CARTESIAN_POINT('',(-18.6658347245569,64.97,-37.7062845255599));
#39375=CARTESIAN_POINT('',(-18.6658347245569,64.97,-37.7062845255599));
#39376=CARTESIAN_POINT('',(-18.7335012750361,64.97,-37.4292696890368));
#39377=CARTESIAN_POINT('',(-18.7335012750361,64.97,-37.4292696890368));
#39378=CARTESIAN_POINT('',(-18.3016633687267,64.97,-36.9020320495254));
#39379=CARTESIAN_POINT('',(-18.3016633687267,64.97,-36.9020320495254));
#39380=CARTESIAN_POINT('',(-17.8521891662412,64.97,-36.4157036251474));
#39381=CARTESIAN_POINT('',(-17.8521891662412,64.97,-36.4157036251474));
#39382=CARTESIAN_POINT('',(-17.3868386222561,64.97,-35.9720703283723));
#39383=CARTESIAN_POINT('',(-17.3868386222561,64.97,-35.9720703283723));
#39384=CARTESIAN_POINT('',(-16.9073260095938,64.97,-35.5733389742151));
#39385=CARTESIAN_POINT('',(-16.9073260095938,64.97,-35.5733389742151));
#39386=CARTESIAN_POINT('',(-16.4152802505257,64.97,-35.2224815976773));
#39387=CARTESIAN_POINT('',(-12.9679083200667,64.97,-34.8397143891372));
#39388=CARTESIAN_POINT('',(-7.38632909621023,64.97,-34.2642224189688));
#39389=CARTESIAN_POINT('',(-13.0625,64.97,-33.));
#39390=CARTESIAN_POINT('',(-13.0625,64.97,-33.));
#39391=CARTESIAN_POINT('',(-12.9679083200667,64.97,-31.1602856108628));
#39392=CARTESIAN_POINT('',(-12.9936165714376,64.97,-31.6602856108628));
#39393=CARTESIAN_POINT('',(-16.3595363724049,64.97,-30.8105898291428));
#39394=CARTESIAN_POINT('',(-6.44552735216333,64.97,-31.8327794916922));
#39395=CARTESIAN_POINT('',(-16.4152802505257,64.97,-30.7775184023227));
#39396=CARTESIAN_POINT('',(-16.4152802505257,64.97,-30.7775184023227));
#39397=CARTESIAN_POINT('',(-16.9073260095938,64.97,-30.4266610257849));
#39398=CARTESIAN_POINT('',(-16.9073260095938,64.97,-30.4266610257849));
#39399=CARTESIAN_POINT('',(-17.3868386222561,64.97,-30.0279296716277));
#39400=CARTESIAN_POINT('',(-17.3868386222561,64.97,-30.0279296716277));
#39401=CARTESIAN_POINT('',(-17.8521891662412,64.97,-29.5842963748526));
#39402=CARTESIAN_POINT('',(-17.8521891662412,64.97,-29.5842963748526));
#39403=CARTESIAN_POINT('',(-18.3016633687267,64.97,-29.0979679504746));
#39404=CARTESIAN_POINT('',(-18.3016633687267,64.97,-29.0979679504746));
#39405=CARTESIAN_POINT('',(-18.7335012750361,64.97,-28.5707303109632));
#39406=CARTESIAN_POINT('',(-18.7335012750361,64.97,-28.5707303109632));
#39407=CARTESIAN_POINT('',(-18.6658347245569,64.97,-28.2937154744401));
#39408=CARTESIAN_POINT('',(-18.6658347245569,64.97,-28.2937154744401));
#39409=CARTESIAN_POINT('',(-18.5940721560646,64.97,-28.0177333817765));
#39410=CARTESIAN_POINT('',(-18.5940721560646,64.97,-28.0177333817765));
#39411=CARTESIAN_POINT('',(-18.518229317088,64.97,-27.742844594294));
#39412=CARTESIAN_POINT('',(-18.518229317088,64.97,-27.742844594294));
#39413=CARTESIAN_POINT('',(-18.4383228505279,64.97,-27.4691094334002));
#39414=CARTESIAN_POINT('',(-18.4383228505279,64.97,-27.4691094334002));
#39415=CARTESIAN_POINT('',(-17.8007214335911,64.97,-27.2284271969067));
#39416=CARTESIAN_POINT('',(-17.8007214335911,64.97,-27.2284271969067));
#39417=CARTESIAN_POINT('',(-17.1683011437039,64.97,-27.0319915280556));
#39418=CARTESIAN_POINT('',(-17.1683011437039,64.97,-27.0319915280556));
#39419=CARTESIAN_POINT('',(-16.5434791025604,64.97,-26.8804690950764));
#39420=CARTESIAN_POINT('',(-16.5434791025604,64.97,-26.8804690950764));
#39421=CARTESIAN_POINT('',(-15.9288433214812,64.97,-26.7749139194219));
#39422=CARTESIAN_POINT('',(-15.9288433214812,64.97,-26.7749139194219));
#39423=CARTESIAN_POINT('',(-15.3272905060348,64.97,-26.7170853977691));
#39424=CARTESIAN_POINT('',(-12.1503952336939,64.97,-28.1092852366672));
#39425=CARTESIAN_POINT('',(-7.02885984751459,64.97,-30.4016841827556));
#39426=CARTESIAN_POINT('',(-11.3124568369342,64.97,-26.46875));
#39427=CARTESIAN_POINT('',(-11.3124568369342,64.97,-26.46875));
#39428=CARTESIAN_POINT('',(-10.3106808445568,64.97,-24.9228064432661));
#39429=CARTESIAN_POINT('',(-10.5829448433309,64.97,-25.3429650194728));
#39430=CARTESIAN_POINT('',(-13.0730690072096,64.97,-22.9241469865312));
#39431=CARTESIAN_POINT('',(-4.99838017360698,64.97,-28.7663937119056));
#39432=CARTESIAN_POINT('',(-13.1048089083576,64.97,-22.8676343517052));
#39433=CARTESIAN_POINT('',(-13.1048089083576,64.97,-22.8676343517052));
#39434=CARTESIAN_POINT('',(-13.3555043472661,64.97,-22.3177600709842));
#39435=CARTESIAN_POINT('',(-13.3555043472661,64.97,-22.3177600709842));
#39436=CARTESIAN_POINT('',(-13.571408774188,64.97,-21.7326922826676));
#39437=CARTESIAN_POINT('',(-13.571408774188,64.97,-21.7326922826676));
#39438=CARTESIAN_POINT('',(-13.7525975185565,64.97,-21.1158193057032));
#39439=CARTESIAN_POINT('',(-13.7525975185565,64.97,-21.1158193057032));
#39440=CARTESIAN_POINT('',(-13.8986893840657,64.97,-20.4699094343666));
#39441=CARTESIAN_POINT('',(-13.8986893840657,64.97,-20.4699094343666));
#39442=CARTESIAN_POINT('',(-14.009053161491,64.97,-19.7973892915637));
#39443=CARTESIAN_POINT('',(-14.009053161491,64.97,-19.7973892915637));
#39444=CARTESIAN_POINT('',(-13.8119447915281,64.97,-19.5913206811491));
#39445=CARTESIAN_POINT('',(-13.8119447915281,64.97,-19.5913206811491));
#39446=CARTESIAN_POINT('',(-13.611805537841,64.97,-19.388194462159));
#39447=CARTESIAN_POINT('',(-13.611805537841,64.97,-19.388194462159));
#39448=CARTESIAN_POINT('',(-13.4086793188509,64.97,-19.1880552084719));
#39449=CARTESIAN_POINT('',(-13.4086793188509,64.97,-19.1880552084719));
#39450=CARTESIAN_POINT('',(-13.2026107084363,64.97,-18.990946838509));
#39451=CARTESIAN_POINT('',(-13.2026107084363,64.97,-18.990946838509));
#39452=CARTESIAN_POINT('',(-12.5300905656334,64.97,-19.1013106159343));
#39453=CARTESIAN_POINT('',(-12.5300905656334,64.97,-19.1013106159343));
#39454=CARTESIAN_POINT('',(-11.8841806942968,64.97,-19.2474024814435));
#39455=CARTESIAN_POINT('',(-11.8841806942968,64.97,-19.2474024814435));
#39456=CARTESIAN_POINT('',(-11.2673077173324,64.97,-19.428591225812));
#39457=CARTESIAN_POINT('',(-11.2673077173324,64.97,-19.428591225812));
#39458=CARTESIAN_POINT('',(-10.6822399290158,64.97,-19.6444956527339));
#39459=CARTESIAN_POINT('',(-10.6822399290158,64.97,-19.6444956527339));
#39460=CARTESIAN_POINT('',(-10.1323656482948,64.97,-19.8951910916424));
#39461=CARTESIAN_POINT('',(-8.07719355673392,64.97,-22.6893191554432));
#39462=CARTESIAN_POINT('',(-4.78801327896586,64.97,-27.2353625714542));
#39463=CARTESIAN_POINT('',(-6.53125,64.97,-21.6875431630658));
#39464=CARTESIAN_POINT('',(-6.53125,64.97,-21.6875431630658));
#39465=CARTESIAN_POINT('',(-4.8907147633328,64.97,-20.8496047663061));
#39466=CARTESIAN_POINT('',(-5.33658159091048,64.97,-21.077340767532));
#39467=CARTESIAN_POINT('',(-6.28368335893612,64.97,-17.7375208219333));
#39468=CARTESIAN_POINT('',(-2.21192106406889,64.97,-26.8343993180852));
#39469=CARTESIAN_POINT('',(-6.28291460223091,64.97,-17.6727094939652));
#39470=CARTESIAN_POINT('',(-6.28291460223091,64.97,-17.6727094939652));
#39471=CARTESIAN_POINT('',(-6.22508608057805,64.97,-17.0711566785188));
#39472=CARTESIAN_POINT('',(-6.22508608057805,64.97,-17.0711566785188));
#39473=CARTESIAN_POINT('',(-6.11953090492364,64.97,-16.4565208974396));
#39474=CARTESIAN_POINT('',(-6.11953090492364,64.97,-16.4565208974396));
#39475=CARTESIAN_POINT('',(-5.96800847194436,64.97,-15.8316988562961));
#39476=CARTESIAN_POINT('',(-5.96800847194436,64.97,-15.8316988562961));
#39477=CARTESIAN_POINT('',(-5.7715728030933,64.97,-15.1992785664089));
#39478=CARTESIAN_POINT('',(-5.7715728030933,64.97,-15.1992785664089));
#39479=CARTESIAN_POINT('',(-5.53089056659976,64.97,-14.5616771494721));
#39480=CARTESIAN_POINT('',(-5.53089056659977,64.97,-14.5616771494721));
#39481=CARTESIAN_POINT('',(-5.25715540570604,64.97,-14.481770682912));
#39482=CARTESIAN_POINT('',(-5.25715540570604,64.97,-14.481770682912));
#39483=CARTESIAN_POINT('',(-4.98226661822352,64.97,-14.4059278439354));
#39484=CARTESIAN_POINT('',(-4.98226661822353,64.97,-14.4059278439354));
#39485=CARTESIAN_POINT('',(-4.70628452555987,64.97,-14.3341652754431));
#39486=CARTESIAN_POINT('',(-4.70628452555987,64.97,-14.3341652754431));
#39487=CARTESIAN_POINT('',(-4.42926968903683,64.97,-14.2664987249639));
#39488=CARTESIAN_POINT('',(-4.42926968903683,64.97,-14.2664987249639));
#39489=CARTESIAN_POINT('',(-3.90203204952539,64.97,-14.6983366312733));
#39490=CARTESIAN_POINT('',(-3.90203204952539,64.97,-14.6983366312733));
#39491=CARTESIAN_POINT('',(-3.4157036251474,64.97,-15.1478108337588));
#39492=CARTESIAN_POINT('',(-3.4157036251474,64.97,-15.1478108337588));
#39493=CARTESIAN_POINT('',(-2.97207032837233,64.97,-15.6131613777439));
#39494=CARTESIAN_POINT('',(-2.97207032837233,64.97,-15.6131613777439));
#39495=CARTESIAN_POINT('',(-2.57333897421511,64.97,-16.0926739904062));
#39496=CARTESIAN_POINT('',(-2.57333897421511,64.97,-16.0926739904062));
#39497=CARTESIAN_POINT('',(-2.22248159767725,64.97,-16.5847197494743));
#39498=CARTESIAN_POINT('',(-1.83971438913717,64.97,-20.0320916799333));
#39499=CARTESIAN_POINT('',(-1.26422241896876,64.97,-25.6136709037898));
#39500=CARTESIAN_POINT('',(1.11022302462516E-15,64.97,-19.9375));
#39501=CARTESIAN_POINT('',(7.99847440693115E-16,64.97,-19.9375));
#39502=CARTESIAN_POINT('',(1.83971438913717,64.97,-20.0320916799333));
#39503=CARTESIAN_POINT('',(1.33971438913717,64.97,-20.0063834285624));
#39504=CARTESIAN_POINT('',(2.18941017085717,64.97,-16.6404636275951));
#39505=CARTESIAN_POINT('',(1.16722050830783,64.97,-26.5544726478367));
#39506=CARTESIAN_POINT('',(2.22248159767725,64.97,-16.5847197494743));
#39507=CARTESIAN_POINT('',(2.22248159767725,64.97,-16.5847197494743));
#39508=CARTESIAN_POINT('',(2.57333897421511,64.97,-16.0926739904062));
#39509=CARTESIAN_POINT('',(2.57333897421511,64.97,-16.0926739904062));
#39510=CARTESIAN_POINT('',(2.97207032837233,64.97,-15.6131613777439));
#39511=CARTESIAN_POINT('',(2.97207032837233,64.97,-15.6131613777439));
#39512=CARTESIAN_POINT('',(3.41570362514739,64.97,-15.1478108337588));
#39513=CARTESIAN_POINT('',(3.41570362514739,64.97,-15.1478108337588));
#39514=CARTESIAN_POINT('',(3.90203204952539,64.97,-14.6983366312733));
#39515=CARTESIAN_POINT('',(3.90203204952539,64.97,-14.6983366312733));
#39516=CARTESIAN_POINT('',(4.42926968903683,64.97,-14.2664987249639));
#39517=CARTESIAN_POINT('',(4.42926968903683,64.97,-14.2664987249639));
#39518=CARTESIAN_POINT('',(4.70628452555987,64.97,-14.3341652754431));
#39519=CARTESIAN_POINT('',(4.70628452555987,64.97,-14.3341652754431));
#39520=CARTESIAN_POINT('',(4.98226661822352,64.97,-14.4059278439354));
#39521=CARTESIAN_POINT('',(4.98226661822352,64.97,-14.4059278439354));
#39522=CARTESIAN_POINT('',(5.25715540570603,64.97,-14.481770682912));
#39523=CARTESIAN_POINT('',(5.25715540570603,64.97,-14.481770682912));
#39524=CARTESIAN_POINT('',(5.53089056659976,64.97,-14.5616771494721));
#39525=CARTESIAN_POINT('',(5.53089056659976,64.97,-14.5616771494721));
#39526=CARTESIAN_POINT('',(5.77157280309329,64.97,-15.1992785664089));
#39527=CARTESIAN_POINT('',(5.77157280309329,64.97,-15.1992785664089));
#39528=CARTESIAN_POINT('',(5.96800847194436,64.97,-15.8316988562961));
#39529=CARTESIAN_POINT('',(5.96800847194436,64.97,-15.8316988562961));
#39530=CARTESIAN_POINT('',(6.11953090492364,64.97,-16.4565208974396));
#39531=CARTESIAN_POINT('',(6.11953090492364,64.97,-16.4565208974396));
#39532=CARTESIAN_POINT('',(6.22508608057805,64.97,-17.0711566785188));
#39533=CARTESIAN_POINT('',(6.22508608057805,64.97,-17.0711566785188));
#39534=CARTESIAN_POINT('',(6.28291460223091,64.97,-17.6727094939652));
#39535=CARTESIAN_POINT('',(-1.04094977927525E-15,64.97,-41.5));
#39536=CARTESIAN_POINT('Origin',(0.,64.97,-33.));
#39537=CARTESIAN_POINT('Origin',(0.918538851438207,64.72,-26.5288321810589));
#39538=CARTESIAN_POINT('',(1.92399462146589,64.7518675845618,-17.0878374925667));
#39539=CARTESIAN_POINT('',(-2.47408096220597,61.1372984587275,-24.5010582960093));
#39540=CARTESIAN_POINT('',(-5.80560826253415,57.3246773483287,-19.6389959268513));
#39541=CARTESIAN_POINT('',(-1.61076884470925,62.0175738804575,-24.7108426070529));
#39542=CARTESIAN_POINT('Origin',(-1.01554076209914,64.72,-25.588030437012));
#39543=CARTESIAN_POINT('',(-1.53371821045904,64.47,-18.1247799404686));
#39544=CARTESIAN_POINT('',(0.0410640680949126,63.4588711803305,-23.5395511505951));
#39545=CARTESIAN_POINT('',(-1.33971438913717,64.47,-20.0063834285624));
#39546=CARTESIAN_POINT('',(-0.766859105229518,64.47,-25.5623899702343));
#39547=CARTESIAN_POINT('',(5.45809628639077,57.6721893244721,-19.6568637773255));
#39548=CARTESIAN_POINT('Origin',(-2.44010592976206,64.72,-26.9365348509256));
#39549=CARTESIAN_POINT('',(-6.28985303478256,64.7518675845618,-18.2576657286835));
#39550=CARTESIAN_POINT('',(-6.39208781628514,61.1372984587275,-26.876741060164));
#39551=CARTESIAN_POINT('',(-11.7083062763497,57.3246773483287,-24.331835183853));
#39552=CARTESIAN_POINT('',(-5.53954543561629,62.0175738804576,-26.6267635440948));
#39553=CARTESIAN_POINT('Origin',(-4.58546888005044,64.72,-27.0888164474249));
#39554=CARTESIAN_POINT('',(-8.76584896227005,64.47,-20.8845406467914));
#39555=CARTESIAN_POINT('',(-4.69466189854939,63.4588711803304,-24.7864789311647));
#39556=CARTESIAN_POINT('',(-7.65703498052716,64.47,-22.4170551566691));
#39557=CARTESIAN_POINT('',(-4.38292448113502,64.47,-26.9422703233957));
#39558=CARTESIAN_POINT('',(-1.94471807102131,57.6721893244721,-18.7154569218122));
#39559=CARTESIAN_POINT('Origin',(-5.14492629763621,64.72,-28.968938110821));
#39560=CARTESIAN_POINT('',(-12.8183396498506,64.7518675845618,-23.3776905273493));
#39561=CARTESIAN_POINT('',(-8.59733990204194,61.1372984587275,-30.8931461122945));
#39562=CARTESIAN_POINT('',(-14.4737730786812,57.3246773483287,-31.3473022032011));
#39563=CARTESIAN_POINT('',(-7.98400530061442,62.0175738804576,-30.2503880426691));
#39564=CARTESIAN_POINT('Origin',(-6.9267243146742,64.72,-30.1734993170625));
#39565=CARTESIAN_POINT('',(-13.6491775636676,64.47,-26.8906289027386));
#39566=CARTESIAN_POINT('',(-8.17245700074035,63.4588711803304,-28.2342130491446));
#39567=CARTESIAN_POINT('',(-11.922659232468,64.47,-27.6634184090895));
#39568=CARTESIAN_POINT('',(-6.8245887818338,64.47,-29.9453144513693));
#39569=CARTESIAN_POINT('',(-8.82644679179704,57.6721893244721,-21.6015818483468));
#39570=CARTESIAN_POINT('Origin',(-6.47116781894107,64.72,-32.0814611485618));
#39571=CARTESIAN_POINT('',(-15.9121625074333,64.7518675845618,-31.0760053785341));
#39572=CARTESIAN_POINT('',(-8.49894170399068,61.1372984587276,-35.4740809622059));
#39573=CARTESIAN_POINT('',(-13.3610040731487,57.3246773483287,-38.8056082625342));
#39574=CARTESIAN_POINT('',(-8.28915739294713,62.0175738804576,-34.6107688447092));
#39575=CARTESIAN_POINT('Origin',(-7.41196956298797,64.72,-34.0155407620991));
#39576=CARTESIAN_POINT('',(-14.8752200595314,64.47,-34.533718210459));
#39577=CARTESIAN_POINT('',(-9.46044884940471,63.4588711803303,-32.9589359319049));
#39578=CARTESIAN_POINT('',(-12.9936165714376,64.47,-34.3397143891372));
#39579=CARTESIAN_POINT('',(-7.43761002976572,64.47,-33.7668591052295));
#39580=CARTESIAN_POINT('',(-13.3431362226745,57.6721893244721,-27.5419037136092));
#39581=CARTESIAN_POINT('Origin',(-6.06346514907441,64.72,-35.4401059297621));
#39582=CARTESIAN_POINT('',(-14.7423342713165,64.7518675845618,-39.2898530347826));
#39583=CARTESIAN_POINT('',(-6.12325893983596,61.1372984587275,-39.3920878162851));
#39584=CARTESIAN_POINT('',(-8.66816481614703,57.3246773483287,-44.7083062763498));
#39585=CARTESIAN_POINT('',(-6.37323645590517,62.0175738804575,-38.5395454356163));
#39586=CARTESIAN_POINT('Origin',(-5.91118355257507,64.72,-37.5854688800504));
#39587=CARTESIAN_POINT('',(-12.1154593532086,64.47,-41.76584896227));
#39588=CARTESIAN_POINT('',(-8.21352106883533,63.4588711803304,-37.6946618985493));
#39589=CARTESIAN_POINT('',(-10.5829448433309,64.47,-40.6570349805272));
#39590=CARTESIAN_POINT('',(-6.0577296766043,64.47,-37.382924481135));
#39591=CARTESIAN_POINT('',(-14.2845430781878,57.6721893244721,-34.9447180710213));
#39592=CARTESIAN_POINT('Origin',(-4.03106188917902,64.72,-38.1449262976362));
#39593=CARTESIAN_POINT('',(-9.62230947265071,64.7518675845618,-45.8183396498506));
#39594=CARTESIAN_POINT('',(-2.10685388770528,61.1372984587272,-41.5973399020421));
#39595=CARTESIAN_POINT('',(-1.65269779679893,57.3246773483287,-47.4737730786812));
#39596=CARTESIAN_POINT('',(-2.74961195733092,62.0175738804576,-40.9840053006144));
#39597=CARTESIAN_POINT('Origin',(-2.82650068293752,64.72,-39.9267243146742));
#39598=CARTESIAN_POINT('',(-6.10937109726139,64.47,-46.6491775636676));
#39599=CARTESIAN_POINT('',(-4.76578695085539,63.4588711803305,-41.1724570007404));
#39600=CARTESIAN_POINT('',(-5.33658159091048,64.47,-44.922659232468));
#39601=CARTESIAN_POINT('',(-3.05468554863069,64.47,-39.8245887818338));
#39602=CARTESIAN_POINT('',(-11.3984181516531,57.6721893244721,-41.826446791797));
#39603=CARTESIAN_POINT('Origin',(-0.918538851438202,64.72,-39.4711678189411));
#39604=CARTESIAN_POINT('',(-1.92399462146589,64.7518675845618,-48.9121625074333));
#39605=CARTESIAN_POINT('',(2.47408096220598,61.1372984587275,-41.4989417039907));
#39606=CARTESIAN_POINT('',(5.80560826253417,57.3246773483287,-46.3610040731487));
#39607=CARTESIAN_POINT('',(1.61076884470942,62.0175738804574,-41.2891573929471));
#39608=CARTESIAN_POINT('Origin',(1.01554076209913,64.72,-40.411969562988));
#39609=CARTESIAN_POINT('',(1.53371821045902,64.47,-47.8752200595314));
#39610=CARTESIAN_POINT('',(-0.0410640680949548,63.4588711803305,-42.4604488494049));
#39611=CARTESIAN_POINT('',(1.33971438913717,64.47,-45.9936165714376));
#39612=CARTESIAN_POINT('',(0.766859105229514,64.47,-40.4376100297657));
#39613=CARTESIAN_POINT('',(-5.45809628639078,57.6721893244721,-46.3431362226745));
#39614=CARTESIAN_POINT('Origin',(2.44010592976207,64.72,-39.0634651490744));
#39615=CARTESIAN_POINT('',(6.28985303478254,64.7518675845618,-47.7423342713165));
#39616=CARTESIAN_POINT('',(6.39208781628516,61.1372984587275,-39.123258939836));
#39617=CARTESIAN_POINT('',(11.7083062763498,57.3246773483287,-41.6681648161471));
#39618=CARTESIAN_POINT('',(5.53954543561639,62.0175738804574,-39.3732364559051));
#39619=CARTESIAN_POINT('Origin',(4.58546888005044,64.72,-38.9111835525751));
#39620=CARTESIAN_POINT('',(8.76584896227005,64.47,-45.1154593532086));
#39621=CARTESIAN_POINT('',(4.6946618985495,63.4588711803305,-41.2135210688354));
#39622=CARTESIAN_POINT('',(7.65703498052716,64.47,-43.5829448433309));
#39623=CARTESIAN_POINT('',(4.38292448113502,64.47,-39.0577296766043));
#39624=CARTESIAN_POINT('',(1.94471807102132,57.6721893244721,-47.2845430781878));
#39625=CARTESIAN_POINT('Origin',(5.1449262976362,64.72,-37.031061889179));
#39626=CARTESIAN_POINT('',(12.8183396498506,64.7518675845618,-42.6223094726507));
#39627=CARTESIAN_POINT('',(8.59733990204205,61.1372984587273,-35.1068538877054));
#39628=CARTESIAN_POINT('',(14.4737730786812,57.3246773483287,-34.6526977967989));
#39629=CARTESIAN_POINT('',(7.98400530061436,62.0175738804577,-35.749611957331));
#39630=CARTESIAN_POINT('Origin',(6.9267243146742,64.72,-35.8265006829375));
#39631=CARTESIAN_POINT('',(13.6491775636676,64.47,-39.1093710972614));
#39632=CARTESIAN_POINT('',(8.17245700074045,63.4588711803305,-37.7657869508554));
#39633=CARTESIAN_POINT('',(11.922659232468,64.47,-38.3365815909105));
#39634=CARTESIAN_POINT('',(6.82458878183381,64.47,-36.0546855486307));
#39635=CARTESIAN_POINT('',(8.82644679179704,57.6721893244721,-44.3984181516532));
#39636=CARTESIAN_POINT('Origin',(6.47116781894107,64.72,-33.9185388514382));
#39637=CARTESIAN_POINT('',(15.9121625074333,64.7518675845618,-34.9239946214659));
#39638=CARTESIAN_POINT('',(8.49894170399068,61.1372984587275,-30.525919037794));
#39639=CARTESIAN_POINT('',(13.3610040731487,57.3246773483287,-27.1943917374658));
#39640=CARTESIAN_POINT('',(8.28915739294707,62.0175738804573,-31.3892311552905));
#39641=CARTESIAN_POINT('Origin',(7.41196956298798,64.72,-31.9844592379009));
#39642=CARTESIAN_POINT('',(14.8752200595314,64.47,-31.466281789541));
#39643=CARTESIAN_POINT('',(9.4604488494049,63.4588711803305,-33.0410640680949));
#39644=CARTESIAN_POINT('',(12.9936165714376,64.47,-31.6602856108628));
#39645=CARTESIAN_POINT('',(7.43761002976572,64.47,-32.2331408947705));
#39646=CARTESIAN_POINT('',(13.3431362226745,57.6721893244721,-38.4580962863908));
#39647=CARTESIAN_POINT('Origin',(6.06346514907441,64.72,-30.5598940702379));
#39648=CARTESIAN_POINT('',(14.7423342713165,64.7518675845618,-26.7101469652175));
#39649=CARTESIAN_POINT('',(6.12325893983594,61.1372984587275,-26.6079121837148));
#39650=CARTESIAN_POINT('',(8.66816481614703,57.3246773483287,-21.2916937236502));
#39651=CARTESIAN_POINT('',(6.37323645590513,62.0175738804575,-27.4604545643837));
#39652=CARTESIAN_POINT('Origin',(5.91118355257506,64.72,-28.4145311199496));
#39653=CARTESIAN_POINT('',(12.1154593532086,64.47,-24.23415103773));
#39654=CARTESIAN_POINT('',(8.21352106883536,63.4588711803305,-28.3053381014505));
#39655=CARTESIAN_POINT('',(10.5829448433309,64.47,-25.3429650194728));
#39656=CARTESIAN_POINT('',(6.05772967660429,64.47,-28.617075518865));
#39657=CARTESIAN_POINT('',(14.2845430781878,57.6721893244721,-31.0552819289787));
#39658=CARTESIAN_POINT('Origin',(4.03106188917902,64.72,-27.8550737023638));
#39659=CARTESIAN_POINT('',(9.62230947265072,64.7518675845618,-20.1816603501494));
#39660=CARTESIAN_POINT('',(2.10685388770537,61.1372984587273,-24.402660097958));
#39661=CARTESIAN_POINT('',(1.65269779679893,57.3246773483287,-18.5262269213188));
#39662=CARTESIAN_POINT('',(2.74961195733085,62.0175738804575,-25.0159946993856));
#39663=CARTESIAN_POINT('Origin',(5.33658159091048,37.03,-21.077340767532));
#39664=CARTESIAN_POINT('',(6.53125,37.03,-21.6875431630658));
#39665=CARTESIAN_POINT('',(5.33658159091048,37.03,-21.077340767532));
#39666=CARTESIAN_POINT('Origin',(6.10937109726139,37.03,-19.3508224363324));
#39667=CARTESIAN_POINT('',(6.10937109726139,37.03,-19.3508224363324));
#39668=CARTESIAN_POINT('Origin',(6.23934797313093,37.03,-18.8210104177224));
#39669=CARTESIAN_POINT('Origin',(6.22508608057805,37.03,-17.0711566785188));
#39670=CARTESIAN_POINT('',(6.22508608057805,37.03,-17.0711566785188));
#39671=CARTESIAN_POINT('Origin',(6.11953090492364,37.03,-16.4565208974396));
#39672=CARTESIAN_POINT('',(6.11953090492364,37.03,-16.4565208974396));
#39673=CARTESIAN_POINT('Origin',(5.96800847194436,37.03,-15.8316988562961));
#39674=CARTESIAN_POINT('',(5.96800847194436,37.03,-15.8316988562961));
#39675=CARTESIAN_POINT('Origin',(5.77157280309329,37.03,-15.1992785664089));
#39676=CARTESIAN_POINT('',(5.77157280309329,37.03,-15.1992785664089));
#39677=CARTESIAN_POINT('Origin',(5.53089056659976,37.03,-14.5616771494721));
#39678=CARTESIAN_POINT('',(5.53089056659976,37.03,-14.5616771494721));
#39679=CARTESIAN_POINT('Origin',(5.25715540570603,37.03,-14.481770682912));
#39680=CARTESIAN_POINT('',(5.25715540570603,37.03,-14.481770682912));
#39681=CARTESIAN_POINT('Origin',(4.98226661822352,37.03,-14.4059278439354));
#39682=CARTESIAN_POINT('',(4.98226661822352,37.03,-14.4059278439354));
#39683=CARTESIAN_POINT('Origin',(4.70628452555987,37.03,-14.3341652754431));
#39684=CARTESIAN_POINT('',(4.70628452555987,37.03,-14.3341652754431));
#39685=CARTESIAN_POINT('Origin',(4.42926968903683,37.03,-14.2664987249639));
#39686=CARTESIAN_POINT('',(4.42926968903683,37.03,-14.2664987249639));
#39687=CARTESIAN_POINT('Origin',(3.90203204952539,37.03,-14.6983366312733));
#39688=CARTESIAN_POINT('',(3.90203204952539,37.03,-14.6983366312733));
#39689=CARTESIAN_POINT('Origin',(3.41570362514739,37.03,-15.1478108337588));
#39690=CARTESIAN_POINT('',(3.41570362514739,37.03,-15.1478108337588));
#39691=CARTESIAN_POINT('Origin',(2.97207032837233,37.03,-15.6131613777439));
#39692=CARTESIAN_POINT('',(2.97207032837233,37.03,-15.6131613777439));
#39693=CARTESIAN_POINT('Origin',(2.57333897421511,37.03,-16.0926739904062));
#39694=CARTESIAN_POINT('',(2.57333897421511,37.03,-16.0926739904062));
#39695=CARTESIAN_POINT('Origin',(2.22248159767725,37.03,-16.5847197494743));
#39696=CARTESIAN_POINT('',(2.22248159767725,37.03,-16.5847197494743));
#39697=CARTESIAN_POINT('Origin',(1.92399462146589,37.03,-17.0878374925667));
#39698=CARTESIAN_POINT('',(1.92399462146589,37.03,-17.0878374925667));
#39699=CARTESIAN_POINT('Origin',(1.68606094335648,37.03,-17.6009608351872));
#39700=CARTESIAN_POINT('Origin',(8.32667268468867E-16,37.03,-19.9375));
#39701=CARTESIAN_POINT('',(7.99847440693115E-16,37.03,-19.9375));
#39702=CARTESIAN_POINT('Origin',(-1.33971438913717,37.03,-20.0063834285624));
#39703=CARTESIAN_POINT('',(-1.33971438913717,37.03,-20.0063834285624));
#39704=CARTESIAN_POINT('Origin',(-1.53371821045904,37.03,-18.1247799404686));
#39705=CARTESIAN_POINT('',(-1.53371821045904,37.03,-18.1247799404686));
#39706=CARTESIAN_POINT('Origin',(-1.68606094335648,37.03,-17.6009608351872));
#39707=CARTESIAN_POINT('Origin',(-2.57333897421511,37.03,-16.0926739904062));
#39708=CARTESIAN_POINT('',(-2.57333897421511,37.03,-16.0926739904062));
#39709=CARTESIAN_POINT('Origin',(-2.97207032837233,37.03,-15.6131613777439));
#39710=CARTESIAN_POINT('',(-2.97207032837233,37.03,-15.6131613777439));
#39711=CARTESIAN_POINT('Origin',(-3.4157036251474,37.03,-15.1478108337588));
#39712=CARTESIAN_POINT('',(-3.4157036251474,37.03,-15.1478108337588));
#39713=CARTESIAN_POINT('Origin',(-3.90203204952539,37.03,-14.6983366312733));
#39714=CARTESIAN_POINT('',(-3.90203204952539,37.03,-14.6983366312733));
#39715=CARTESIAN_POINT('Origin',(-4.42926968903683,37.03,-14.2664987249639));
#39716=CARTESIAN_POINT('',(-4.42926968903683,37.03,-14.2664987249639));
#39717=CARTESIAN_POINT('Origin',(-4.70628452555987,37.03,-14.3341652754431));
#39718=CARTESIAN_POINT('',(-4.70628452555987,37.03,-14.3341652754431));
#39719=CARTESIAN_POINT('Origin',(-4.98226661822353,37.03,-14.4059278439354));
#39720=CARTESIAN_POINT('',(-4.98226661822353,37.03,-14.4059278439354));
#39721=CARTESIAN_POINT('Origin',(-5.25715540570604,37.03,-14.481770682912));
#39722=CARTESIAN_POINT('',(-5.25715540570604,37.03,-14.481770682912));
#39723=CARTESIAN_POINT('Origin',(-5.53089056659977,37.03,-14.5616771494721));
#39724=CARTESIAN_POINT('',(-5.53089056659977,37.03,-14.5616771494721));
#39725=CARTESIAN_POINT('Origin',(-5.7715728030933,37.03,-15.1992785664089));
#39726=CARTESIAN_POINT('',(-5.7715728030933,37.03,-15.1992785664089));
#39727=CARTESIAN_POINT('Origin',(-5.96800847194436,37.03,-15.8316988562961));
#39728=CARTESIAN_POINT('',(-5.96800847194436,37.03,-15.8316988562961));
#39729=CARTESIAN_POINT('Origin',(-6.11953090492364,37.03,-16.4565208974396));
#39730=CARTESIAN_POINT('',(-6.11953090492364,37.03,-16.4565208974396));
#39731=CARTESIAN_POINT('Origin',(-6.22508608057805,37.03,-17.0711566785188));
#39732=CARTESIAN_POINT('',(-6.22508608057805,37.03,-17.0711566785188));
#39733=CARTESIAN_POINT('Origin',(-6.28291460223091,37.03,-17.6727094939652));
#39734=CARTESIAN_POINT('',(-6.28291460223091,37.03,-17.6727094939652));
#39735=CARTESIAN_POINT('Origin',(-6.28985303478256,37.03,-18.2576657286835));
#39736=CARTESIAN_POINT('',(-6.28985303478256,37.03,-18.2576657286835));
#39737=CARTESIAN_POINT('Origin',(-6.23934797313094,37.03,-18.8210104177224));
#39738=CARTESIAN_POINT('Origin',(-6.53125,37.03,-21.6875431630658));
#39739=CARTESIAN_POINT('',(-6.53125,37.03,-21.6875431630658));
#39740=CARTESIAN_POINT('Origin',(-7.65703498052716,37.03,-22.4170551566691));
#39741=CARTESIAN_POINT('',(-7.65703498052716,37.03,-22.4170551566691));
#39742=CARTESIAN_POINT('Origin',(-8.76584896227005,37.03,-20.8845406467914));
#39743=CARTESIAN_POINT('',(-8.76584896227005,37.03,-20.8845406467914));
#39744=CARTESIAN_POINT('Origin',(-9.15969119168187,37.03,-20.5070713610788));
#39745=CARTESIAN_POINT('Origin',(-10.6822399290158,37.03,-19.6444956527339));
#39746=CARTESIAN_POINT('',(-10.6822399290158,37.03,-19.6444956527339));
#39747=CARTESIAN_POINT('Origin',(-11.2673077173324,37.03,-19.428591225812));
#39748=CARTESIAN_POINT('',(-11.2673077173324,37.03,-19.428591225812));
#39749=CARTESIAN_POINT('Origin',(-11.8841806942968,37.03,-19.2474024814435));
#39750=CARTESIAN_POINT('',(-11.8841806942968,37.03,-19.2474024814435));
#39751=CARTESIAN_POINT('Origin',(-12.5300905656334,37.03,-19.1013106159343));
#39752=CARTESIAN_POINT('',(-12.5300905656334,37.03,-19.1013106159343));
#39753=CARTESIAN_POINT('Origin',(-13.2026107084363,37.03,-18.990946838509));
#39754=CARTESIAN_POINT('',(-13.2026107084363,37.03,-18.990946838509));
#39755=CARTESIAN_POINT('Origin',(-13.4086793188509,37.03,-19.1880552084719));
#39756=CARTESIAN_POINT('',(-13.4086793188509,37.03,-19.1880552084719));
#39757=CARTESIAN_POINT('Origin',(-13.611805537841,37.03,-19.388194462159));
#39758=CARTESIAN_POINT('',(-13.611805537841,37.03,-19.388194462159));
#39759=CARTESIAN_POINT('Origin',(-13.8119447915281,37.03,-19.5913206811491));
#39760=CARTESIAN_POINT('',(-13.8119447915281,37.03,-19.5913206811491));
#39761=CARTESIAN_POINT('Origin',(-14.009053161491,37.03,-19.7973892915637));
#39762=CARTESIAN_POINT('',(-14.009053161491,37.03,-19.7973892915637));
#39763=CARTESIAN_POINT('Origin',(-13.8986893840657,37.03,-20.4699094343666));
#39764=CARTESIAN_POINT('',(-13.8986893840657,37.03,-20.4699094343666));
#39765=CARTESIAN_POINT('Origin',(-13.7525975185565,37.03,-21.1158193057032));
#39766=CARTESIAN_POINT('',(-13.7525975185565,37.03,-21.1158193057032));
#39767=CARTESIAN_POINT('Origin',(-13.571408774188,37.03,-21.7326922826676));
#39768=CARTESIAN_POINT('',(-13.571408774188,37.03,-21.7326922826676));
#39769=CARTESIAN_POINT('Origin',(-13.3555043472661,37.03,-22.3177600709842));
#39770=CARTESIAN_POINT('',(-13.3555043472661,37.03,-22.3177600709842));
#39771=CARTESIAN_POINT('Origin',(-13.1048089083576,37.03,-22.8676343517052));
#39772=CARTESIAN_POINT('',(-13.1048089083576,37.03,-22.8676343517052));
#39773=CARTESIAN_POINT('Origin',(-12.8183396498506,37.03,-23.3776905273493));
#39774=CARTESIAN_POINT('',(-12.8183396498506,37.03,-23.3776905273493));
#39775=CARTESIAN_POINT('Origin',(-12.4929286389212,37.03,-23.8403088083181));
#39776=CARTESIAN_POINT('Origin',(-11.3124568369342,37.03,-26.46875));
#39777=CARTESIAN_POINT('',(-11.3124568369342,37.03,-26.46875));
#39778=CARTESIAN_POINT('Origin',(-11.922659232468,37.03,-27.6634184090895));
#39779=CARTESIAN_POINT('',(-11.922659232468,37.03,-27.6634184090895));
#39780=CARTESIAN_POINT('Origin',(-13.6491775636676,37.03,-26.8906289027386));
#39781=CARTESIAN_POINT('',(-13.6491775636676,37.03,-26.8906289027386));
#39782=CARTESIAN_POINT('Origin',(-14.1789895822776,37.03,-26.7606520268691));
#39783=CARTESIAN_POINT('Origin',(-15.9288433214812,37.03,-26.7749139194219));
#39784=CARTESIAN_POINT('',(-15.9288433214812,37.03,-26.7749139194219));
#39785=CARTESIAN_POINT('Origin',(-16.5434791025604,37.03,-26.8804690950764));
#39786=CARTESIAN_POINT('',(-16.5434791025604,37.03,-26.8804690950764));
#39787=CARTESIAN_POINT('Origin',(-17.1683011437039,37.03,-27.0319915280556));
#39788=CARTESIAN_POINT('',(-17.1683011437039,37.03,-27.0319915280556));
#39789=CARTESIAN_POINT('Origin',(-17.8007214335911,37.03,-27.2284271969067));
#39790=CARTESIAN_POINT('',(-17.8007214335911,37.03,-27.2284271969067));
#39791=CARTESIAN_POINT('Origin',(-18.4383228505279,37.03,-27.4691094334002));
#39792=CARTESIAN_POINT('',(-18.4383228505279,37.03,-27.4691094334002));
#39793=CARTESIAN_POINT('Origin',(-18.518229317088,37.03,-27.742844594294));
#39794=CARTESIAN_POINT('',(-18.518229317088,37.03,-27.742844594294));
#39795=CARTESIAN_POINT('Origin',(-18.5940721560646,37.03,-28.0177333817765));
#39796=CARTESIAN_POINT('',(-18.5940721560646,37.03,-28.0177333817765));
#39797=CARTESIAN_POINT('Origin',(-18.6658347245569,37.03,-28.2937154744401));
#39798=CARTESIAN_POINT('',(-18.6658347245569,37.03,-28.2937154744401));
#39799=CARTESIAN_POINT('Origin',(-18.7335012750361,37.03,-28.5707303109632));
#39800=CARTESIAN_POINT('',(-18.7335012750361,37.03,-28.5707303109632));
#39801=CARTESIAN_POINT('Origin',(-18.3016633687267,37.03,-29.0979679504746));
#39802=CARTESIAN_POINT('',(-18.3016633687267,37.03,-29.0979679504746));
#39803=CARTESIAN_POINT('Origin',(-17.8521891662412,37.03,-29.5842963748526));
#39804=CARTESIAN_POINT('',(-17.8521891662412,37.03,-29.5842963748526));
#39805=CARTESIAN_POINT('Origin',(-17.3868386222561,37.03,-30.0279296716277));
#39806=CARTESIAN_POINT('',(-17.3868386222561,37.03,-30.0279296716277));
#39807=CARTESIAN_POINT('Origin',(-16.9073260095938,37.03,-30.4266610257849));
#39808=CARTESIAN_POINT('',(-16.9073260095938,37.03,-30.4266610257849));
#39809=CARTESIAN_POINT('Origin',(-16.4152802505257,37.03,-30.7775184023227));
#39810=CARTESIAN_POINT('',(-16.4152802505257,37.03,-30.7775184023227));
#39811=CARTESIAN_POINT('Origin',(-15.9121625074333,37.03,-31.0760053785341));
#39812=CARTESIAN_POINT('',(-15.9121625074333,37.03,-31.0760053785341));
#39813=CARTESIAN_POINT('Origin',(-15.3990391648128,37.03,-31.3139390566435));
#39814=CARTESIAN_POINT('Origin',(-13.0625,37.03,-33.));
#39815=CARTESIAN_POINT('',(-13.0625,37.03,-33.));
#39816=CARTESIAN_POINT('Origin',(-12.9936165714376,37.03,-34.3397143891372));
#39817=CARTESIAN_POINT('',(-12.9936165714376,37.03,-34.3397143891372));
#39818=CARTESIAN_POINT('Origin',(-14.8752200595314,37.03,-34.533718210459));
#39819=CARTESIAN_POINT('',(-14.8752200595314,37.03,-34.533718210459));
#39820=CARTESIAN_POINT('Origin',(-15.3990391648128,37.03,-34.6860609433565));
#39821=CARTESIAN_POINT('Origin',(-16.9073260095938,37.03,-35.5733389742151));
#39822=CARTESIAN_POINT('',(-16.9073260095938,37.03,-35.5733389742151));
#39823=CARTESIAN_POINT('Origin',(-17.3868386222561,37.03,-35.9720703283723));
#39824=CARTESIAN_POINT('',(-17.3868386222561,37.03,-35.9720703283723));
#39825=CARTESIAN_POINT('Origin',(-17.8521891662412,37.03,-36.4157036251474));
#39826=CARTESIAN_POINT('',(-17.8521891662412,37.03,-36.4157036251474));
#39827=CARTESIAN_POINT('Origin',(-18.3016633687267,37.03,-36.9020320495254));
#39828=CARTESIAN_POINT('',(-18.3016633687267,37.03,-36.9020320495254));
#39829=CARTESIAN_POINT('Origin',(-18.7335012750361,37.03,-37.4292696890368));
#39830=CARTESIAN_POINT('',(-18.7335012750361,37.03,-37.4292696890368));
#39831=CARTESIAN_POINT('Origin',(-18.6658347245569,37.03,-37.7062845255599));
#39832=CARTESIAN_POINT('',(-18.6658347245569,37.03,-37.7062845255599));
#39833=CARTESIAN_POINT('Origin',(-18.5940721560646,37.03,-37.9822666182235));
#39834=CARTESIAN_POINT('',(-18.5940721560646,37.03,-37.9822666182235));
#39835=CARTESIAN_POINT('Origin',(-18.518229317088,37.03,-38.257155405706));
#39836=CARTESIAN_POINT('',(-18.518229317088,37.03,-38.257155405706));
#39837=CARTESIAN_POINT('Origin',(-18.4383228505279,37.03,-38.5308905665998));
#39838=CARTESIAN_POINT('',(-18.4383228505279,37.03,-38.5308905665998));
#39839=CARTESIAN_POINT('Origin',(-17.8007214335911,37.03,-38.7715728030933));
#39840=CARTESIAN_POINT('',(-17.8007214335911,37.03,-38.7715728030933));
#39841=CARTESIAN_POINT('Origin',(-17.1683011437039,37.03,-38.9680084719444));
#39842=CARTESIAN_POINT('',(-17.1683011437039,37.03,-38.9680084719444));
#39843=CARTESIAN_POINT('Origin',(-16.5434791025604,37.03,-39.1195309049236));
#39844=CARTESIAN_POINT('',(-16.5434791025604,37.03,-39.1195309049236));
#39845=CARTESIAN_POINT('Origin',(-15.9288433214812,37.03,-39.225086080578));
#39846=CARTESIAN_POINT('',(-15.9288433214812,37.03,-39.225086080578));
#39847=CARTESIAN_POINT('Origin',(-15.3272905060348,37.03,-39.2829146022309));
#39848=CARTESIAN_POINT('',(-15.3272905060348,37.03,-39.2829146022309));
#39849=CARTESIAN_POINT('Origin',(-14.7423342713165,37.03,-39.2898530347826));
#39850=CARTESIAN_POINT('',(-14.7423342713165,37.03,-39.2898530347826));
#39851=CARTESIAN_POINT('Origin',(-14.1789895822776,37.03,-39.2393479731309));
#39852=CARTESIAN_POINT('Origin',(-11.3124568369342,37.03,-39.53125));
#39853=CARTESIAN_POINT('',(-11.3124568369342,37.03,-39.53125));
#39854=CARTESIAN_POINT('Origin',(-10.5829448433309,37.03,-40.6570349805272));
#39855=CARTESIAN_POINT('',(-10.5829448433309,37.03,-40.6570349805272));
#39856=CARTESIAN_POINT('Origin',(-12.1154593532086,37.03,-41.76584896227));
#39857=CARTESIAN_POINT('',(-12.1154593532086,37.03,-41.76584896227));
#39858=CARTESIAN_POINT('Origin',(-12.4929286389212,37.03,-42.1596911916819));
#39859=CARTESIAN_POINT('Origin',(-13.3555043472661,37.03,-43.6822399290158));
#39860=CARTESIAN_POINT('',(-13.3555043472661,37.03,-43.6822399290158));
#39861=CARTESIAN_POINT('Origin',(-13.571408774188,37.03,-44.2673077173324));
#39862=CARTESIAN_POINT('',(-13.571408774188,37.03,-44.2673077173324));
#39863=CARTESIAN_POINT('Origin',(-13.7525975185565,37.03,-44.8841806942968));
#39864=CARTESIAN_POINT('',(-13.7525975185565,37.03,-44.8841806942968));
#39865=CARTESIAN_POINT('Origin',(-13.8986893840657,37.03,-45.5300905656334));
#39866=CARTESIAN_POINT('',(-13.8986893840657,37.03,-45.5300905656334));
#39867=CARTESIAN_POINT('Origin',(-14.009053161491,37.03,-46.2026107084363));
#39868=CARTESIAN_POINT('',(-14.009053161491,37.03,-46.2026107084363));
#39869=CARTESIAN_POINT('Origin',(-13.8119447915281,37.03,-46.4086793188509));
#39870=CARTESIAN_POINT('',(-13.8119447915281,37.03,-46.4086793188509));
#39871=CARTESIAN_POINT('Origin',(-13.611805537841,37.03,-46.611805537841));
#39872=CARTESIAN_POINT('',(-13.611805537841,37.03,-46.611805537841));
#39873=CARTESIAN_POINT('Origin',(-13.4086793188509,37.03,-46.8119447915281));
#39874=CARTESIAN_POINT('',(-13.4086793188509,37.03,-46.8119447915281));
#39875=CARTESIAN_POINT('Origin',(-13.2026107084363,37.03,-47.009053161491));
#39876=CARTESIAN_POINT('',(-13.2026107084363,37.03,-47.009053161491));
#39877=CARTESIAN_POINT('Origin',(-12.5300905656334,37.03,-46.8986893840657));
#39878=CARTESIAN_POINT('',(-12.5300905656334,37.03,-46.8986893840657));
#39879=CARTESIAN_POINT('Origin',(-11.8841806942968,37.03,-46.7525975185565));
#39880=CARTESIAN_POINT('',(-11.8841806942968,37.03,-46.7525975185565));
#39881=CARTESIAN_POINT('Origin',(-11.2673077173324,37.03,-46.571408774188));
#39882=CARTESIAN_POINT('',(-11.2673077173324,37.03,-46.571408774188));
#39883=CARTESIAN_POINT('Origin',(-10.6822399290158,37.03,-46.3555043472661));
#39884=CARTESIAN_POINT('',(-10.6822399290158,37.03,-46.3555043472661));
#39885=CARTESIAN_POINT('Origin',(-10.1323656482948,37.03,-46.1048089083576));
#39886=CARTESIAN_POINT('',(-10.1323656482948,37.03,-46.1048089083576));
#39887=CARTESIAN_POINT('Origin',(-9.62230947265071,37.03,-45.8183396498506));
#39888=CARTESIAN_POINT('',(-9.62230947265071,37.03,-45.8183396498506));
#39889=CARTESIAN_POINT('Origin',(-9.15969119168187,37.03,-45.4929286389212));
#39890=CARTESIAN_POINT('Origin',(-6.53125000000001,37.03,-44.3124568369342));
#39891=CARTESIAN_POINT('',(-6.53125000000001,37.03,-44.3124568369342));
#39892=CARTESIAN_POINT('Origin',(-5.33658159091048,37.03,-44.922659232468));
#39893=CARTESIAN_POINT('',(-5.33658159091048,37.03,-44.922659232468));
#39894=CARTESIAN_POINT('Origin',(-6.10937109726139,37.03,-46.6491775636676));
#39895=CARTESIAN_POINT('',(-6.10937109726139,37.03,-46.6491775636676));
#39896=CARTESIAN_POINT('Origin',(-6.23934797313094,37.03,-47.1789895822776));
#39897=CARTESIAN_POINT('Origin',(-6.22508608057804,37.03,-48.9288433214812));
#39898=CARTESIAN_POINT('',(-6.22508608057804,37.03,-48.9288433214812));
#39899=CARTESIAN_POINT('Origin',(-6.11953090492364,37.03,-49.5434791025604));
#39900=CARTESIAN_POINT('',(-6.11953090492364,37.03,-49.5434791025604));
#39901=CARTESIAN_POINT('Origin',(-5.96800847194436,37.03,-50.1683011437039));
#39902=CARTESIAN_POINT('',(-5.96800847194436,37.03,-50.1683011437039));
#39903=CARTESIAN_POINT('Origin',(-5.7715728030933,37.03,-50.8007214335911));
#39904=CARTESIAN_POINT('',(-5.7715728030933,37.03,-50.8007214335911));
#39905=CARTESIAN_POINT('Origin',(-5.53089056659976,37.03,-51.4383228505279));
#39906=CARTESIAN_POINT('',(-5.53089056659976,37.03,-51.4383228505279));
#39907=CARTESIAN_POINT('Origin',(-5.25715540570604,37.03,-51.518229317088));
#39908=CARTESIAN_POINT('',(-5.25715540570604,37.03,-51.518229317088));
#39909=CARTESIAN_POINT('Origin',(-4.98226661822352,37.03,-51.5940721560646));
#39910=CARTESIAN_POINT('',(-4.98226661822352,37.03,-51.5940721560646));
#39911=CARTESIAN_POINT('Origin',(-4.70628452555985,37.03,-51.6658347245569));
#39912=CARTESIAN_POINT('',(-4.70628452555985,37.03,-51.6658347245569));
#39913=CARTESIAN_POINT('Origin',(-4.42926968903682,37.03,-51.7335012750361));
#39914=CARTESIAN_POINT('',(-4.42926968903682,37.03,-51.7335012750361));
#39915=CARTESIAN_POINT('Origin',(-3.90203204952539,37.03,-51.3016633687267));
#39916=CARTESIAN_POINT('',(-3.90203204952539,37.03,-51.3016633687267));
#39917=CARTESIAN_POINT('Origin',(-3.41570362514739,37.03,-50.8521891662412));
#39918=CARTESIAN_POINT('',(-3.41570362514739,37.03,-50.8521891662412));
#39919=CARTESIAN_POINT('Origin',(-2.97207032837234,37.03,-50.3868386222561));
#39920=CARTESIAN_POINT('',(-2.97207032837234,37.03,-50.3868386222561));
#39921=CARTESIAN_POINT('Origin',(-2.57333897421511,37.03,-49.9073260095938));
#39922=CARTESIAN_POINT('',(-2.57333897421511,37.03,-49.9073260095938));
#39923=CARTESIAN_POINT('Origin',(-2.22248159767726,37.03,-49.4152802505257));
#39924=CARTESIAN_POINT('',(-2.22248159767726,37.03,-49.4152802505257));
#39925=CARTESIAN_POINT('Origin',(-1.92399462146589,37.03,-48.9121625074333));
#39926=CARTESIAN_POINT('',(-1.92399462146589,37.03,-48.9121625074333));
#39927=CARTESIAN_POINT('Origin',(-1.68606094335648,37.03,-48.3990391648128));
#39928=CARTESIAN_POINT('Origin',(-2.4980018054066E-15,37.03,-46.0625));
#39929=CARTESIAN_POINT('',(-2.39954232207934E-15,37.03,-46.0625));
#39930=CARTESIAN_POINT('Origin',(1.33971438913717,37.03,-45.9936165714376));
#39931=CARTESIAN_POINT('',(1.33971438913717,37.03,-45.9936165714376));
#39932=CARTESIAN_POINT('Origin',(1.53371821045902,37.03,-47.8752200595314));
#39933=CARTESIAN_POINT('',(1.53371821045902,37.03,-47.8752200595314));
#39934=CARTESIAN_POINT('Origin',(1.68606094335647,37.03,-48.3990391648128));
#39935=CARTESIAN_POINT('Origin',(2.57333897421511,37.03,-49.9073260095938));
#39936=CARTESIAN_POINT('',(2.57333897421511,37.03,-49.9073260095938));
#39937=CARTESIAN_POINT('Origin',(2.97207032837233,37.03,-50.3868386222561));
#39938=CARTESIAN_POINT('',(2.97207032837233,37.03,-50.3868386222561));
#39939=CARTESIAN_POINT('Origin',(3.41570362514738,37.03,-50.8521891662412));
#39940=CARTESIAN_POINT('',(3.41570362514738,37.03,-50.8521891662412));
#39941=CARTESIAN_POINT('Origin',(3.90203204952538,37.03,-51.3016633687267));
#39942=CARTESIAN_POINT('',(3.90203204952538,37.03,-51.3016633687267));
#39943=CARTESIAN_POINT('Origin',(4.42926968903682,37.03,-51.7335012750361));
#39944=CARTESIAN_POINT('',(4.42926968903682,37.03,-51.7335012750361));
#39945=CARTESIAN_POINT('Origin',(4.70628452555985,37.03,-51.6658347245569));
#39946=CARTESIAN_POINT('',(4.70628452555985,37.03,-51.6658347245569));
#39947=CARTESIAN_POINT('Origin',(4.98226661822352,37.03,-51.5940721560646));
#39948=CARTESIAN_POINT('',(4.98226661822352,37.03,-51.5940721560646));
#39949=CARTESIAN_POINT('Origin',(5.25715540570603,37.03,-51.518229317088));
#39950=CARTESIAN_POINT('',(5.25715540570603,37.03,-51.518229317088));
#39951=CARTESIAN_POINT('Origin',(5.53089056659975,37.03,-51.4383228505279));
#39952=CARTESIAN_POINT('',(5.53089056659975,37.03,-51.4383228505279));
#39953=CARTESIAN_POINT('Origin',(5.77157280309329,37.03,-50.8007214335911));
#39954=CARTESIAN_POINT('',(5.77157280309329,37.03,-50.8007214335911));
#39955=CARTESIAN_POINT('Origin',(5.96800847194436,37.03,-50.1683011437039));
#39956=CARTESIAN_POINT('',(5.96800847194436,37.03,-50.1683011437039));
#39957=CARTESIAN_POINT('Origin',(6.11953090492363,37.03,-49.5434791025604));
#39958=CARTESIAN_POINT('',(6.11953090492363,37.03,-49.5434791025604));
#39959=CARTESIAN_POINT('Origin',(6.22508608057804,37.03,-48.9288433214812));
#39960=CARTESIAN_POINT('',(6.22508608057804,37.03,-48.9288433214812));
#39961=CARTESIAN_POINT('Origin',(6.2829146022309,37.03,-48.3272905060348));
#39962=CARTESIAN_POINT('',(6.2829146022309,37.03,-48.3272905060348));
#39963=CARTESIAN_POINT('Origin',(6.28985303478254,37.03,-47.7423342713165));
#39964=CARTESIAN_POINT('',(6.28985303478254,37.03,-47.7423342713165));
#39965=CARTESIAN_POINT('Origin',(6.23934797313093,37.03,-47.1789895822776));
#39966=CARTESIAN_POINT('Origin',(6.53125,37.03,-44.3124568369342));
#39967=CARTESIAN_POINT('',(6.53125,37.03,-44.3124568369342));
#39968=CARTESIAN_POINT('Origin',(7.65703498052716,37.03,-43.5829448433309));
#39969=CARTESIAN_POINT('',(7.65703498052716,37.03,-43.5829448433309));
#39970=CARTESIAN_POINT('Origin',(8.76584896227005,37.03,-45.1154593532086));
#39971=CARTESIAN_POINT('',(8.76584896227005,37.03,-45.1154593532086));
#39972=CARTESIAN_POINT('Origin',(9.15969119168186,37.03,-45.4929286389212));
#39973=CARTESIAN_POINT('Origin',(10.6822399290158,37.03,-46.3555043472661));
#39974=CARTESIAN_POINT('',(10.6822399290158,37.03,-46.3555043472661));
#39975=CARTESIAN_POINT('Origin',(11.2673077173324,37.03,-46.571408774188));
#39976=CARTESIAN_POINT('',(11.2673077173324,37.03,-46.571408774188));
#39977=CARTESIAN_POINT('Origin',(11.8841806942968,37.03,-46.7525975185565));
#39978=CARTESIAN_POINT('',(11.8841806942968,37.03,-46.7525975185565));
#39979=CARTESIAN_POINT('Origin',(12.5300905656334,37.03,-46.8986893840657));
#39980=CARTESIAN_POINT('',(12.5300905656334,37.03,-46.8986893840657));
#39981=CARTESIAN_POINT('Origin',(13.2026107084363,37.03,-47.009053161491));
#39982=CARTESIAN_POINT('',(13.2026107084363,37.03,-47.009053161491));
#39983=CARTESIAN_POINT('Origin',(13.4086793188509,37.03,-46.8119447915281));
#39984=CARTESIAN_POINT('',(13.4086793188509,37.03,-46.8119447915281));
#39985=CARTESIAN_POINT('Origin',(13.611805537841,37.03,-46.6118055378411));
#39986=CARTESIAN_POINT('',(13.611805537841,37.03,-46.6118055378411));
#39987=CARTESIAN_POINT('Origin',(13.8119447915281,37.03,-46.4086793188509));
#39988=CARTESIAN_POINT('',(13.8119447915281,37.03,-46.4086793188509));
#39989=CARTESIAN_POINT('Origin',(14.009053161491,37.03,-46.2026107084364));
#39990=CARTESIAN_POINT('',(14.009053161491,37.03,-46.2026107084364));
#39991=CARTESIAN_POINT('Origin',(13.8986893840657,37.03,-45.5300905656334));
#39992=CARTESIAN_POINT('',(13.8986893840657,37.03,-45.5300905656334));
#39993=CARTESIAN_POINT('Origin',(13.7525975185565,37.03,-44.8841806942968));
#39994=CARTESIAN_POINT('',(13.7525975185565,37.03,-44.8841806942968));
#39995=CARTESIAN_POINT('Origin',(13.571408774188,37.03,-44.2673077173324));
#39996=CARTESIAN_POINT('',(13.571408774188,37.03,-44.2673077173324));
#39997=CARTESIAN_POINT('Origin',(13.3555043472661,37.03,-43.6822399290158));
#39998=CARTESIAN_POINT('',(13.3555043472661,37.03,-43.6822399290158));
#39999=CARTESIAN_POINT('Origin',(13.1048089083576,37.03,-43.1323656482948));
#40000=CARTESIAN_POINT('',(13.1048089083576,37.03,-43.1323656482948));
#40001=CARTESIAN_POINT('Origin',(12.8183396498506,37.03,-42.6223094726507));
#40002=CARTESIAN_POINT('',(12.8183396498506,37.03,-42.6223094726507));
#40003=CARTESIAN_POINT('Origin',(12.4929286389212,37.03,-42.1596911916819));
#40004=CARTESIAN_POINT('Origin',(11.3124568369342,37.03,-39.53125));
#40005=CARTESIAN_POINT('',(11.3124568369342,37.03,-39.53125));
#40006=CARTESIAN_POINT('Origin',(11.922659232468,37.03,-38.3365815909105));
#40007=CARTESIAN_POINT('',(11.922659232468,37.03,-38.3365815909105));
#40008=CARTESIAN_POINT('Origin',(13.6491775636676,37.03,-39.1093710972614));
#40009=CARTESIAN_POINT('',(13.6491775636676,37.03,-39.1093710972614));
#40010=CARTESIAN_POINT('Origin',(14.1789895822776,37.03,-39.2393479731309));
#40011=CARTESIAN_POINT('Origin',(15.9288433214812,37.03,-39.225086080578));
#40012=CARTESIAN_POINT('',(15.9288433214812,37.03,-39.225086080578));
#40013=CARTESIAN_POINT('Origin',(16.5434791025604,37.03,-39.1195309049236));
#40014=CARTESIAN_POINT('',(16.5434791025604,37.03,-39.1195309049236));
#40015=CARTESIAN_POINT('Origin',(17.1683011437039,37.03,-38.9680084719444));
#40016=CARTESIAN_POINT('',(17.1683011437039,37.03,-38.9680084719444));
#40017=CARTESIAN_POINT('Origin',(17.8007214335911,37.03,-38.7715728030933));
#40018=CARTESIAN_POINT('',(17.8007214335911,37.03,-38.7715728030933));
#40019=CARTESIAN_POINT('Origin',(18.4383228505279,37.03,-38.5308905665998));
#40020=CARTESIAN_POINT('',(18.4383228505279,37.03,-38.5308905665998));
#40021=CARTESIAN_POINT('Origin',(18.518229317088,37.03,-38.257155405706));
#40022=CARTESIAN_POINT('',(18.518229317088,37.03,-38.257155405706));
#40023=CARTESIAN_POINT('Origin',(18.5940721560646,37.03,-37.9822666182235));
#40024=CARTESIAN_POINT('',(18.5940721560646,37.03,-37.9822666182235));
#40025=CARTESIAN_POINT('Origin',(18.6658347245569,37.03,-37.7062845255599));
#40026=CARTESIAN_POINT('',(18.6658347245569,37.03,-37.7062845255599));
#40027=CARTESIAN_POINT('Origin',(18.7335012750361,37.03,-37.4292696890368));
#40028=CARTESIAN_POINT('',(18.7335012750361,37.03,-37.4292696890368));
#40029=CARTESIAN_POINT('Origin',(18.3016633687267,37.03,-36.9020320495254));
#40030=CARTESIAN_POINT('',(18.3016633687267,37.03,-36.9020320495254));
#40031=CARTESIAN_POINT('Origin',(17.8521891662412,37.03,-36.4157036251474));
#40032=CARTESIAN_POINT('',(17.8521891662412,37.03,-36.4157036251474));
#40033=CARTESIAN_POINT('Origin',(17.3868386222561,37.03,-35.9720703283723));
#40034=CARTESIAN_POINT('',(17.3868386222561,37.03,-35.9720703283723));
#40035=CARTESIAN_POINT('Origin',(16.9073260095938,37.03,-35.5733389742151));
#40036=CARTESIAN_POINT('',(16.9073260095938,37.03,-35.5733389742151));
#40037=CARTESIAN_POINT('Origin',(16.4152802505257,37.03,-35.2224815976773));
#40038=CARTESIAN_POINT('',(16.4152802505257,37.03,-35.2224815976773));
#40039=CARTESIAN_POINT('Origin',(15.9121625074333,37.03,-34.9239946214659));
#40040=CARTESIAN_POINT('',(15.9121625074333,37.03,-34.9239946214659));
#40041=CARTESIAN_POINT('Origin',(15.3990391648128,37.03,-34.6860609433565));
#40042=CARTESIAN_POINT('Origin',(13.0625,37.03,-33.));
#40043=CARTESIAN_POINT('',(13.0625,37.03,-33.));
#40044=CARTESIAN_POINT('Origin',(12.9936165714376,37.03,-31.6602856108628));
#40045=CARTESIAN_POINT('',(12.9936165714376,37.03,-31.6602856108628));
#40046=CARTESIAN_POINT('Origin',(14.8752200595314,37.03,-31.466281789541));
#40047=CARTESIAN_POINT('',(14.8752200595314,37.03,-31.466281789541));
#40048=CARTESIAN_POINT('Origin',(15.3990391648128,37.03,-31.3139390566435));
#40049=CARTESIAN_POINT('Origin',(16.9073260095938,37.03,-30.4266610257849));
#40050=CARTESIAN_POINT('',(16.9073260095938,37.03,-30.4266610257849));
#40051=CARTESIAN_POINT('Origin',(17.3868386222561,37.03,-30.0279296716277));
#40052=CARTESIAN_POINT('',(17.3868386222561,37.03,-30.0279296716277));
#40053=CARTESIAN_POINT('Origin',(17.8521891662412,37.03,-29.5842963748526));
#40054=CARTESIAN_POINT('',(17.8521891662412,37.03,-29.5842963748526));
#40055=CARTESIAN_POINT('Origin',(18.3016633687267,37.03,-29.0979679504746));
#40056=CARTESIAN_POINT('',(18.3016633687267,37.03,-29.0979679504746));
#40057=CARTESIAN_POINT('Origin',(18.7335012750361,37.03,-28.5707303109632));
#40058=CARTESIAN_POINT('',(18.7335012750361,37.03,-28.5707303109632));
#40059=CARTESIAN_POINT('Origin',(18.6658347245569,37.03,-28.2937154744402));
#40060=CARTESIAN_POINT('',(18.6658347245569,37.03,-28.2937154744402));
#40061=CARTESIAN_POINT('Origin',(18.5940721560646,37.03,-28.0177333817765));
#40062=CARTESIAN_POINT('',(18.5940721560646,37.03,-28.0177333817765));
#40063=CARTESIAN_POINT('Origin',(18.518229317088,37.03,-27.742844594294));
#40064=CARTESIAN_POINT('',(18.518229317088,37.03,-27.742844594294));
#40065=CARTESIAN_POINT('Origin',(18.4383228505279,37.03,-27.4691094334002));
#40066=CARTESIAN_POINT('',(18.4383228505279,37.03,-27.4691094334002));
#40067=CARTESIAN_POINT('Origin',(17.8007214335911,37.03,-27.2284271969067));
#40068=CARTESIAN_POINT('',(17.8007214335911,37.03,-27.2284271969067));
#40069=CARTESIAN_POINT('Origin',(17.1683011437039,37.03,-27.0319915280556));
#40070=CARTESIAN_POINT('',(17.1683011437039,37.03,-27.0319915280556));
#40071=CARTESIAN_POINT('Origin',(16.5434791025604,37.03,-26.8804690950764));
#40072=CARTESIAN_POINT('',(16.5434791025604,37.03,-26.8804690950764));
#40073=CARTESIAN_POINT('Origin',(15.9288433214812,37.03,-26.774913919422));
#40074=CARTESIAN_POINT('',(15.9288433214812,37.03,-26.774913919422));
#40075=CARTESIAN_POINT('Origin',(15.3272905060348,37.03,-26.7170853977691));
#40076=CARTESIAN_POINT('',(15.3272905060348,37.03,-26.7170853977691));
#40077=CARTESIAN_POINT('Origin',(14.7423342713165,37.03,-26.7101469652175));
#40078=CARTESIAN_POINT('',(14.7423342713165,37.03,-26.7101469652175));
#40079=CARTESIAN_POINT('Origin',(14.1789895822776,37.03,-26.7606520268691));
#40080=CARTESIAN_POINT('Origin',(11.3124568369342,37.03,-26.46875));
#40081=CARTESIAN_POINT('',(11.3124568369342,37.03,-26.46875));
#40082=CARTESIAN_POINT('Origin',(10.5829448433309,37.03,-25.3429650194728));
#40083=CARTESIAN_POINT('',(10.5829448433309,37.03,-25.3429650194728));
#40084=CARTESIAN_POINT('Origin',(12.1154593532086,37.03,-24.23415103773));
#40085=CARTESIAN_POINT('',(12.1154593532086,37.03,-24.23415103773));
#40086=CARTESIAN_POINT('Origin',(12.4929286389212,37.03,-23.8403088083181));
#40087=CARTESIAN_POINT('Origin',(13.3555043472661,37.03,-22.3177600709842));
#40088=CARTESIAN_POINT('',(13.3555043472661,37.03,-22.3177600709842));
#40089=CARTESIAN_POINT('Origin',(13.571408774188,37.03,-21.7326922826676));
#40090=CARTESIAN_POINT('',(13.571408774188,37.03,-21.7326922826676));
#40091=CARTESIAN_POINT('Origin',(13.7525975185565,37.03,-21.1158193057032));
#40092=CARTESIAN_POINT('',(13.7525975185565,37.03,-21.1158193057032));
#40093=CARTESIAN_POINT('Origin',(13.8986893840657,37.03,-20.4699094343666));
#40094=CARTESIAN_POINT('',(13.8986893840657,37.03,-20.4699094343666));
#40095=CARTESIAN_POINT('Origin',(14.009053161491,37.03,-19.7973892915637));
#40096=CARTESIAN_POINT('',(14.009053161491,37.03,-19.7973892915637));
#40097=CARTESIAN_POINT('Origin',(13.8119447915281,37.03,-19.5913206811491));
#40098=CARTESIAN_POINT('',(13.8119447915281,37.03,-19.5913206811491));
#40099=CARTESIAN_POINT('Origin',(13.611805537841,37.03,-19.388194462159));
#40100=CARTESIAN_POINT('',(13.611805537841,37.03,-19.388194462159));
#40101=CARTESIAN_POINT('Origin',(13.4086793188509,37.03,-19.1880552084719));
#40102=CARTESIAN_POINT('',(13.4086793188509,37.03,-19.1880552084719));
#40103=CARTESIAN_POINT('Origin',(13.2026107084364,37.03,-18.990946838509));
#40104=CARTESIAN_POINT('',(13.2026107084364,37.03,-18.990946838509));
#40105=CARTESIAN_POINT('Origin',(12.5300905656334,37.03,-19.1013106159343));
#40106=CARTESIAN_POINT('',(12.5300905656334,37.03,-19.1013106159343));
#40107=CARTESIAN_POINT('Origin',(11.8841806942968,37.03,-19.2474024814435));
#40108=CARTESIAN_POINT('',(11.8841806942968,37.03,-19.2474024814435));
#40109=CARTESIAN_POINT('Origin',(11.2673077173324,37.03,-19.428591225812));
#40110=CARTESIAN_POINT('',(11.2673077173324,37.03,-19.428591225812));
#40111=CARTESIAN_POINT('Origin',(10.6822399290158,37.03,-19.6444956527339));
#40112=CARTESIAN_POINT('',(10.6822399290158,37.03,-19.6444956527339));
#40113=CARTESIAN_POINT('Origin',(10.1323656482948,37.03,-19.8951910916424));
#40114=CARTESIAN_POINT('',(10.1323656482948,37.03,-19.8951910916424));
#40115=CARTESIAN_POINT('Origin',(9.62230947265072,37.03,-20.1816603501494));
#40116=CARTESIAN_POINT('',(9.62230947265072,37.03,-20.1816603501494));
#40117=CARTESIAN_POINT('Origin',(9.15969119168187,37.03,-20.5070713610788));
#40118=CARTESIAN_POINT('Origin',(6.53125,37.03,-21.6875431630658));
#40119=CARTESIAN_POINT('Origin',(0.,51.,-33.));
#40120=CARTESIAN_POINT('',(-1.04094977927525E-15,18.05,-41.5));
#40121=CARTESIAN_POINT('',(-1.04094977927525E-15,51.,-41.5));
#40122=CARTESIAN_POINT('Origin',(0.,18.05,-33.));
#40123=CARTESIAN_POINT('Origin',(0.,18.05,-24.5));
#40124=CARTESIAN_POINT('Origin',(0.,51.,-33.));
#40125=CARTESIAN_POINT('',(-1.04094977927525E-15,83.95,-41.5));
#40126=CARTESIAN_POINT('Origin',(0.,83.95,-33.));
#40127=CARTESIAN_POINT('',(-1.04094977927525E-15,51.,-41.5));
#40128=CARTESIAN_POINT('Origin',(0.,83.95,-33.));
#40129=CARTESIAN_POINT('',(0.,0.,0.));
#40130=CARTESIAN_POINT('Origin',(9.,37.,-12.));
#40131=CARTESIAN_POINT('',(9.,37.,-12.));
#40132=CARTESIAN_POINT('',(3.,37.,-12.));
#40133=CARTESIAN_POINT('',(4.5,37.,-12.));
#40134=CARTESIAN_POINT('',(9.,36.2,-12.));
#40135=CARTESIAN_POINT('',(9.,37.,-12.));
#40136=CARTESIAN_POINT('',(3.,36.2,-12.));
#40137=CARTESIAN_POINT('',(3.,36.2,-12.));
#40138=CARTESIAN_POINT('',(3.,37.,-12.));
#40139=CARTESIAN_POINT('Origin',(9.,37.,-21.));
#40140=CARTESIAN_POINT('',(9.,37.,-21.));
#40141=CARTESIAN_POINT('',(9.,37.,-18.75));
#40142=CARTESIAN_POINT('',(9.,36.2,-21.));
#40143=CARTESIAN_POINT('',(9.,37.,-21.));
#40144=CARTESIAN_POINT('',(9.,36.2,-12.));
#40145=CARTESIAN_POINT('Origin',(3.,37.,-21.));
#40146=CARTESIAN_POINT('',(3.,37.,-21.));
#40147=CARTESIAN_POINT('',(1.5,37.,-21.));
#40148=CARTESIAN_POINT('',(3.,36.2,-21.));
#40149=CARTESIAN_POINT('',(3.,37.,-21.));
#40150=CARTESIAN_POINT('',(9.,36.2,-21.));
#40151=CARTESIAN_POINT('Origin',(3.,37.,-12.));
#40152=CARTESIAN_POINT('',(3.,37.,-14.25));
#40153=CARTESIAN_POINT('',(3.,36.2,-21.));
#40154=CARTESIAN_POINT('Origin',(6.,36.2,-16.5));
#40155=CARTESIAN_POINT('Origin',(-9.,37.,-12.));
#40156=CARTESIAN_POINT('',(-9.,37.,-12.));
#40157=CARTESIAN_POINT('',(-9.,37.,-21.));
#40158=CARTESIAN_POINT('',(-9.,37.,-14.25));
#40159=CARTESIAN_POINT('',(-9.,36.2,-12.));
#40160=CARTESIAN_POINT('',(-9.,37.,-12.));
#40161=CARTESIAN_POINT('',(-9.,36.2,-21.));
#40162=CARTESIAN_POINT('',(-9.,36.2,-12.));
#40163=CARTESIAN_POINT('',(-9.,37.,-21.));
#40164=CARTESIAN_POINT('Origin',(-3.,37.,-12.));
#40165=CARTESIAN_POINT('',(-3.,37.,-12.));
#40166=CARTESIAN_POINT('',(-1.5,37.,-12.));
#40167=CARTESIAN_POINT('',(-3.,36.2,-12.));
#40168=CARTESIAN_POINT('',(-3.,37.,-12.));
#40169=CARTESIAN_POINT('',(-3.,36.2,-12.));
#40170=CARTESIAN_POINT('Origin',(-3.,37.,-21.));
#40171=CARTESIAN_POINT('',(-3.,37.,-21.));
#40172=CARTESIAN_POINT('',(-3.,37.,-18.75));
#40173=CARTESIAN_POINT('',(-3.,36.2,-21.));
#40174=CARTESIAN_POINT('',(-3.,37.,-21.));
#40175=CARTESIAN_POINT('',(-3.,36.2,-21.));
#40176=CARTESIAN_POINT('Origin',(-9.,37.,-21.));
#40177=CARTESIAN_POINT('',(-4.5,37.,-21.));
#40178=CARTESIAN_POINT('',(-9.,36.2,-21.));
#40179=CARTESIAN_POINT('Origin',(-6.,36.2,-16.5));
#40180=CARTESIAN_POINT('Origin',(0.,18.,0.));
#40181=CARTESIAN_POINT('',(-11.5,18.,1.40834381901946E-15));
#40182=CARTESIAN_POINT('Origin',(0.,18.,0.));
#40183=CARTESIAN_POINT('',(-11.5,37.,1.40834381901946E-15));
#40184=CARTESIAN_POINT('',(-11.5,18.,1.40834381901946E-15));
#40185=CARTESIAN_POINT('Origin',(0.,37.,0.));
#40186=CARTESIAN_POINT('Origin',(0.,18.,-33.));
#40187=CARTESIAN_POINT('',(-11.5,18.,-33.));
#40188=CARTESIAN_POINT('Origin',(0.,18.,-33.));
#40189=CARTESIAN_POINT('',(-11.5,37.,-33.));
#40190=CARTESIAN_POINT('',(-11.5,18.,-33.));
#40191=CARTESIAN_POINT('Origin',(0.,37.,-33.));
#40192=CARTESIAN_POINT('Origin',(0.,18.,0.));
#40193=CARTESIAN_POINT('',(-9.91526600752597,18.,-16.5));
#40194=CARTESIAN_POINT('',(9.91526600752597,18.,-16.5));
#40195=CARTESIAN_POINT('Origin',(0.,18.,0.));
#40196=CARTESIAN_POINT('',(9.91526600752597,37.,-16.5));
#40197=CARTESIAN_POINT('',(9.91526600752597,18.,-16.5));
#40198=CARTESIAN_POINT('',(-9.91526600752597,37.,-16.5));
#40199=CARTESIAN_POINT('Origin',(0.,37.,0.));
#40200=CARTESIAN_POINT('',(-9.91526600752597,18.,-16.5));
#40201=CARTESIAN_POINT('Origin',(0.,18.,-33.));
#40202=CARTESIAN_POINT('Origin',(0.,18.,-33.));
#40203=CARTESIAN_POINT('Origin',(0.,37.,-33.));
#40204=CARTESIAN_POINT('Origin',(0.,37.,-16.5));
#40205=CARTESIAN_POINT('Origin',(0.,18.,-16.5));
#40206=CARTESIAN_POINT('',(0.,0.,0.));
#40207=CARTESIAN_POINT('Origin',(0.0762138451062111,0.,-2.96920392492399E-16));
#40208=CARTESIAN_POINT('',(0.152427690212422,9.69815599727615,-1.18768156996959E-15));
#40209=CARTESIAN_POINT('',(0.152427690212421,-9.69815599727615,-1.18768156996959E-15));
#40210=CARTESIAN_POINT('Origin',(0.152427690212422,0.,-5.93840784984797E-16));
#40211=CARTESIAN_POINT('Origin',(0.152427690212422,0.,-5.93840784984797E-16));
#40212=CARTESIAN_POINT('',(0.,9.25,1.1327982892113E-15));
#40213=CARTESIAN_POINT('',(0.0762138451062111,9.47407799863807,1.16023992959045E-15));
#40214=CARTESIAN_POINT('Origin',(0.,0.,0.));
#40215=CARTESIAN_POINT('Origin',(0.,9.5,0.));
#40216=CARTESIAN_POINT('',(0.,-7.94,-9.72369558522999E-16));
#40217=CARTESIAN_POINT('Origin',(0.,0.,0.));
#40218=CARTESIAN_POINT('Origin',(0.5,0.,0.));
#40219=CARTESIAN_POINT('',(1.,-10.8,-1.32261854307914E-15));
#40220=CARTESIAN_POINT('Origin',(1.,0.,0.));
#40221=CARTESIAN_POINT('',(0.5,-10.15,-1.24301650113456E-15));
#40222=CARTESIAN_POINT('Origin',(1.5,0.,0.));
#40223=CARTESIAN_POINT('',(3.,-7.94,-9.72369558522999E-16));
#40224=CARTESIAN_POINT('Origin',(3.,0.,0.));
#40225=CARTESIAN_POINT('',(1.5,-7.94,-9.72369558522999E-16));
#40226=CARTESIAN_POINT('Origin',(1.,14.29,0.));
#40227=CARTESIAN_POINT('',(1.,-14.29,-1.75002027598157E-15));
#40228=CARTESIAN_POINT('Origin',(1.,0.,0.));
#40229=CARTESIAN_POINT('Origin',(3.675,0.,0.));
#40230=CARTESIAN_POINT('',(6.35,-14.29,-1.75002027598157E-15));
#40231=CARTESIAN_POINT('Origin',(6.35,0.,0.));
#40232=CARTESIAN_POINT('',(3.675,-14.29,-1.75002027598157E-15));
#40233=CARTESIAN_POINT('Origin',(6.35,12.,0.));
#40234=CARTESIAN_POINT('',(6.35,-12.,-1.46957615897682E-15));
#40235=CARTESIAN_POINT('Origin',(6.35,0.,0.));
#40236=CARTESIAN_POINT('Origin',(5.675,0.,0.));
#40237=CARTESIAN_POINT('',(5.,-12.,-1.46957615897682E-15));
#40238=CARTESIAN_POINT('',(5.675,-12.,-1.46957615897682E-15));
#40239=CARTESIAN_POINT('Origin',(5.,0.,0.));
#40240=CARTESIAN_POINT('Origin',(5.,10.2,0.));
#40241=CARTESIAN_POINT('',(5.,-10.2,-1.2491397351303E-15));
#40242=CARTESIAN_POINT('Origin',(5.,0.,0.));
#40243=CARTESIAN_POINT('Origin',(4.,0.,0.));
#40244=CARTESIAN_POINT('',(4.,-9.07,-1.11075464682665E-15));
#40245=CARTESIAN_POINT('',(0.,0.,0.));
#40246=CARTESIAN_POINT('Origin',(1.1,-3.1,5.83535368620123));
#40247=CARTESIAN_POINT('',(1.,-3.,11.8253963992756));
#40248=CARTESIAN_POINT('',(1.,-3.,14.3906219462537));
#40249=CARTESIAN_POINT('',(1.,-3.,5.83535368620123));
#40250=CARTESIAN_POINT('',(1.2,-3.2,14.3474736452102));
#40251=CARTESIAN_POINT('Origin',(-2.00000000000001,1.08246744900953E-14,
1.38777878078145E-16));
#40252=CARTESIAN_POINT('',(1.2,-3.2,11.9799833054975));
#40253=CARTESIAN_POINT('',(1.2,-3.2,5.83535368620123));
#40254=CARTESIAN_POINT('Ctrl Pts',(1.2,-3.2,11.9799833054975));
#40255=CARTESIAN_POINT('Ctrl Pts',(1.13323634243527,-3.13323634243527,11.928712311713));
#40256=CARTESIAN_POINT('Ctrl Pts',(1.06656451099022,-3.06656451099022,11.8771826972087));
#40257=CARTESIAN_POINT('Ctrl Pts',(1.,-3.,11.8253963992756));
#40258=CARTESIAN_POINT('Origin',(1.1,-2.77555756156289E-16,-4.5102810375397E-16));
#40259=CARTESIAN_POINT('',(1.,3.,11.8253963992756));
#40260=CARTESIAN_POINT('Origin',(1.,-2.77555756156289E-16,-4.5102810375397E-16));
#40261=CARTESIAN_POINT('',(1.2,3.2,11.9799833054975));
#40262=CARTESIAN_POINT('Origin',(1.2,-2.77555756156289E-16,-4.5102810375397E-16));
#40263=CARTESIAN_POINT('Ctrl Pts',(1.2,3.2,11.9799833054975));
#40264=CARTESIAN_POINT('Ctrl Pts',(1.13323634243556,3.13323634243555,11.9287123117132));
#40265=CARTESIAN_POINT('Ctrl Pts',(1.06656451099035,3.06656451099035,11.8771826972088));
#40266=CARTESIAN_POINT('Ctrl Pts',(1.,3.,11.8253963992756));
#40267=CARTESIAN_POINT('Origin',(1.1,3.1,7.11796645969031));
#40268=CARTESIAN_POINT('',(1.2,3.2,14.3474736452102));
#40269=CARTESIAN_POINT('',(1.2,3.2,7.11796645969031));
#40270=CARTESIAN_POINT('',(1.,3.,14.3906219462537));
#40271=CARTESIAN_POINT('Origin',(-1.99999999999999,1.08246744900953E-14,
1.38777878078145E-16));
#40272=CARTESIAN_POINT('',(1.,3.,7.11796645969031));
#40273=CARTESIAN_POINT('Origin',(0.,-3.,11.8253963992756));
#40274=CARTESIAN_POINT('',(0.2,-3.,11.8253963992756));
#40275=CARTESIAN_POINT('',(0.,-3.,11.8253963992756));
#40276=CARTESIAN_POINT('',(0.2,-3.,14.3906219462537));
#40277=CARTESIAN_POINT('',(0.2,-3.,5.83535368620123));
#40278=CARTESIAN_POINT('',(0.,-3.,14.3906219462537));
#40279=CARTESIAN_POINT('Origin',(0.,-2.77555756156289E-16,-4.5102810375397E-16));
#40280=CARTESIAN_POINT('',(0.2,3.,11.8253963992756));
#40281=CARTESIAN_POINT('',(0.,3.,11.8253963992756));
#40282=CARTESIAN_POINT('Origin',(0.2,-2.77555756156289E-16,-4.5102810375397E-16));
#40283=CARTESIAN_POINT('Origin',(0.,3.,14.3906219462537));
#40284=CARTESIAN_POINT('',(0.2,3.,14.3906219462537));
#40285=CARTESIAN_POINT('',(0.,3.,14.3906219462537));
#40286=CARTESIAN_POINT('',(0.2,3.,7.11796645969031));
#40287=CARTESIAN_POINT('Origin',(0.1,3.1,7.11796645969031));
#40288=CARTESIAN_POINT('',(0.,3.2,14.3474736452102));
#40289=CARTESIAN_POINT('Origin',(3.19999999999999,1.08246744900953E-14,
1.38777878078145E-16));
#40290=CARTESIAN_POINT('',(0.,3.2,11.9799833054975));
#40291=CARTESIAN_POINT('',(0.,3.2,7.11796645969031));
#40292=CARTESIAN_POINT('Ctrl Pts',(8.15320033709099E-16,3.2,11.9799833054975));
#40293=CARTESIAN_POINT('Ctrl Pts',(0.0667636575643691,3.13323634243563,
11.9287123117132));
#40294=CARTESIAN_POINT('Ctrl Pts',(0.133435489009609,3.06656451099039,11.8771826972088));
#40295=CARTESIAN_POINT('Ctrl Pts',(0.2,3.,11.8253963992756));
#40296=CARTESIAN_POINT('Origin',(0.1,-2.77555756156289E-16,-4.5102810375397E-16));
#40297=CARTESIAN_POINT('',(0.,-3.2,11.9799833054975));
#40298=CARTESIAN_POINT('Origin',(0.,-2.77555756156289E-16,-4.5102810375397E-16));
#40299=CARTESIAN_POINT('Ctrl Pts',(-1.07552855510562E-15,-3.2,11.9799833054975));
#40300=CARTESIAN_POINT('Ctrl Pts',(0.06676365756418,-3.13323634243582,11.9287123117134));
#40301=CARTESIAN_POINT('Ctrl Pts',(0.133435489009517,-3.06656451099048,
11.8771826972089));
#40302=CARTESIAN_POINT('Ctrl Pts',(0.199999999999999,-3.,11.8253963992756));
#40303=CARTESIAN_POINT('Origin',(0.1,-3.1,5.83535368620123));
#40304=CARTESIAN_POINT('',(0.,-3.2,14.3474736452102));
#40305=CARTESIAN_POINT('',(0.,-3.2,5.83535368620123));
#40306=CARTESIAN_POINT('Origin',(3.20000000000001,1.08246744900953E-14,
1.38777878078145E-16));
#40307=CARTESIAN_POINT('Origin',(0.,1.11022302462516E-14,-0.154689026873125));
#40308=CARTESIAN_POINT('Origin',(0.,1.08246744900953E-14,1.38777878078145E-16));
#40309=CARTESIAN_POINT('',(0.,-4.5,13.67));
#40310=CARTESIAN_POINT('Origin',(0.,-4.5,12.67));
#40311=CARTESIAN_POINT('',(0.,4.5,13.67));
#40312=CARTESIAN_POINT('Origin',(0.,4.5,12.67));
#40313=CARTESIAN_POINT('Origin',(0.,1.08246744900953E-14,1.38777878078145E-16));
#40314=CARTESIAN_POINT('Origin',(1.2,1.08246744900953E-14,1.38777878078145E-16));
#40315=CARTESIAN_POINT('Origin',(0.1,-4.5,12.67));
#40316=CARTESIAN_POINT('',(0.2,-4.5,13.47));
#40317=CARTESIAN_POINT('',(0.1,-4.5,13.57));
#40318=CARTESIAN_POINT('Origin',(0.2,-4.5,12.67));
#40319=CARTESIAN_POINT('Origin',(-0.1,-4.5,12.67));
#40320=CARTESIAN_POINT('',(1.,-4.5,13.47));
#40321=CARTESIAN_POINT('',(-0.1,-4.5,13.47));
#40322=CARTESIAN_POINT('Origin',(1.,-4.5,12.67));
#40323=CARTESIAN_POINT('Origin',(1.1,-4.5,12.67));
#40324=CARTESIAN_POINT('',(1.2,-4.5,13.67));
#40325=CARTESIAN_POINT('Origin',(1.2,-4.5,12.67));
#40326=CARTESIAN_POINT('',(1.1,-4.5,13.57));
#40327=CARTESIAN_POINT('Origin',(1.2,1.11022302462516E-14,-0.154689026873125));
#40328=CARTESIAN_POINT('',(1.2,4.5,13.67));
#40329=CARTESIAN_POINT('Origin',(1.2,4.5,12.67));
#40330=CARTESIAN_POINT('Origin',(0.1,4.5,12.67));
#40331=CARTESIAN_POINT('',(0.2,4.5,13.47));
#40332=CARTESIAN_POINT('',(0.1,4.5,13.57));
#40333=CARTESIAN_POINT('Origin',(0.2,4.5,12.67));
#40334=CARTESIAN_POINT('Origin',(-0.1,4.5,12.67));
#40335=CARTESIAN_POINT('',(1.,4.5,13.47));
#40336=CARTESIAN_POINT('',(-0.1,4.5,13.47));
#40337=CARTESIAN_POINT('Origin',(1.,4.5,12.67));
#40338=CARTESIAN_POINT('Origin',(1.1,4.5,12.67));
#40339=CARTESIAN_POINT('',(1.1,4.5,13.57));
#40340=CARTESIAN_POINT('',(0.,0.,0.));
#40341=CARTESIAN_POINT('Origin',(1.885,-34.8,8.9275));
#40342=CARTESIAN_POINT('',(1.86,-34.825,9.795));
#40343=CARTESIAN_POINT('',(1.785,-34.9,9.72));
#40344=CARTESIAN_POINT('',(1.25666666666667,-35.4283333333333,9.19166666666666));
#40345=CARTESIAN_POINT('',(1.785,-34.9,6.15));
#40346=CARTESIAN_POINT('',(1.785,-34.9,8.9275));
#40347=CARTESIAN_POINT('',(1.86,-34.825,6.075));
#40348=CARTESIAN_POINT('',(1.25666666666667,-35.4283333333333,6.67833333333333));
#40349=CARTESIAN_POINT('',(1.985,-34.7,6.2));
#40350=CARTESIAN_POINT('',(2.33125,-34.35375,6.54625));
#40351=CARTESIAN_POINT('',(1.985,-34.7,9.67));
#40352=CARTESIAN_POINT('',(1.985,-34.7,8.9275));
#40353=CARTESIAN_POINT('',(2.00041666666667,-34.6845833333333,9.65458333333333));
#40354=CARTESIAN_POINT('Origin',(1.985,-34.9,9.92));
#40355=CARTESIAN_POINT('',(1.985,-10.3,6.2));
#40356=CARTESIAN_POINT('',(1.985,-34.9,6.2));
#40357=CARTESIAN_POINT('',(1.985,-10.3,9.67));
#40358=CARTESIAN_POINT('',(1.985,-10.3,8.9275));
#40359=CARTESIAN_POINT('',(1.985,-34.9,9.67));
#40360=CARTESIAN_POINT('Origin',(1.86,-34.9,6.075));
#40361=CARTESIAN_POINT('',(1.735,-34.7,5.95));
#40362=CARTESIAN_POINT('',(1.71958333333333,-34.6845833333333,5.93458333333333));
#40363=CARTESIAN_POINT('',(1.735,-10.3,5.95));
#40364=CARTESIAN_POINT('',(1.735,-34.9,5.95));
#40365=CARTESIAN_POINT('',(1.86,-10.175,6.075));
#40366=CARTESIAN_POINT('',(-2.41375000000001,-14.4487500000001,1.80124999999999));
#40367=CARTESIAN_POINT('',(6.46458333333334,-14.7795833333334,10.6795833333333));
#40368=CARTESIAN_POINT('Origin',(0.9925,-34.8,6.05));
#40369=CARTESIAN_POINT('',(-1.785,-34.9,6.15));
#40370=CARTESIAN_POINT('',(0.9925,-34.9,6.15));
#40371=CARTESIAN_POINT('',(-1.86,-34.825,6.075));
#40372=CARTESIAN_POINT('',(-1.25666666666667,-35.4283333333333,6.67833333333333));
#40373=CARTESIAN_POINT('',(-1.735,-34.7,5.95));
#40374=CARTESIAN_POINT('',(-1.38875,-34.35375,5.60375));
#40375=CARTESIAN_POINT('',(0.9925,-34.7,5.95));
#40376=CARTESIAN_POINT('Origin',(-1.885,-34.8,6.9425));
#40377=CARTESIAN_POINT('',(-1.785,-34.9,9.72));
#40378=CARTESIAN_POINT('',(-1.785,-34.9,6.9425));
#40379=CARTESIAN_POINT('',(-1.86,-34.825,9.795));
#40380=CARTESIAN_POINT('',(-1.25666666666667,-35.4283333333333,9.19166666666667));
#40381=CARTESIAN_POINT('',(-1.985,-34.7,9.67));
#40382=CARTESIAN_POINT('',(-2.33125,-34.35375,9.32375));
#40383=CARTESIAN_POINT('',(-1.985,-34.7,6.2));
#40384=CARTESIAN_POINT('',(-1.985,-34.7,6.9425));
#40385=CARTESIAN_POINT('',(-2.00041666666667,-34.6845833333333,6.21541666666666));
#40386=CARTESIAN_POINT('Origin',(-1.985,-34.9,5.95));
#40387=CARTESIAN_POINT('',(-1.985,-10.3,9.67));
#40388=CARTESIAN_POINT('',(-1.985,-34.9,9.67));
#40389=CARTESIAN_POINT('',(-1.985,-10.3,6.2));
#40390=CARTESIAN_POINT('',(-1.985,-10.3,6.9425));
#40391=CARTESIAN_POINT('',(-1.985,-34.9,6.2));
#40392=CARTESIAN_POINT('Origin',(-1.86,-34.9,9.795));
#40393=CARTESIAN_POINT('',(-1.735,-34.7,9.92));
#40394=CARTESIAN_POINT('',(-1.71958333333333,-34.6845833333333,9.93541666666667));
#40395=CARTESIAN_POINT('',(-1.735,-10.3,9.92));
#40396=CARTESIAN_POINT('',(-1.735,-34.9,9.92));
#40397=CARTESIAN_POINT('',(-1.86,-10.175,9.795));
#40398=CARTESIAN_POINT('',(2.41375000000001,-14.4487500000001,14.06875));
#40399=CARTESIAN_POINT('',(-6.46458333333334,-14.7795833333334,5.19041666666666));
#40400=CARTESIAN_POINT('Origin',(-0.9925,-34.8,9.82));
#40401=CARTESIAN_POINT('',(1.735,-34.7,9.92));
#40402=CARTESIAN_POINT('',(1.38875,-34.35375,10.26625));
#40403=CARTESIAN_POINT('',(-0.9925,-34.7,9.92));
#40404=CARTESIAN_POINT('',(-0.9925,-34.9,9.72));
#40405=CARTESIAN_POINT('Origin',(1.985,-34.9,5.95));
#40406=CARTESIAN_POINT('',(-1.735,-10.3,5.95));
#40407=CARTESIAN_POINT('',(-1.735,-34.9,5.95));
#40408=CARTESIAN_POINT('',(0.9925,-10.3,5.95));
#40409=CARTESIAN_POINT('Origin',(-1.885,-10.2,6.9425));
#40410=CARTESIAN_POINT('',(-1.785,-10.1,9.72));
#40411=CARTESIAN_POINT('',(-1.25666666666667,-9.57166666666666,9.19166666666667));
#40412=CARTESIAN_POINT('',(-1.785,-10.1,6.15));
#40413=CARTESIAN_POINT('',(-1.785,-10.1,6.9425));
#40414=CARTESIAN_POINT('',(-1.86,-10.175,6.075));
#40415=CARTESIAN_POINT('',(-1.25666666666667,-9.57166666666666,6.67833333333333));
#40416=CARTESIAN_POINT('',(-6.13375000000003,-14.4487500000001,10.34875));
#40417=CARTESIAN_POINT('Origin',(0.9925,-10.2,6.05));
#40418=CARTESIAN_POINT('',(1.785,-10.1,6.15));
#40419=CARTESIAN_POINT('',(0.9925,-10.1,6.15));
#40420=CARTESIAN_POINT('',(1.25666666666667,-9.57166666666666,6.67833333333333));
#40421=CARTESIAN_POINT('',(2.74458333333335,-14.7795833333334,1.47041666666667));
#40422=CARTESIAN_POINT('Origin',(0.,-10.1,7.935));
#40423=CARTESIAN_POINT('',(1.785,-10.1,9.72));
#40424=CARTESIAN_POINT('',(-0.9925,-10.1,9.72));
#40425=CARTESIAN_POINT('',(1.785,-10.1,8.9275));
#40426=CARTESIAN_POINT('Origin',(-0.9925,-10.2,9.82));
#40427=CARTESIAN_POINT('',(1.735,-10.3,9.92));
#40428=CARTESIAN_POINT('',(-0.9925,-10.3,9.92));
#40429=CARTESIAN_POINT('',(1.86,-10.175,9.795));
#40430=CARTESIAN_POINT('',(-2.74458333333335,-14.7795833333334,14.3995833333333));
#40431=CARTESIAN_POINT('',(1.25666666666667,-9.57166666666666,9.19166666666667));
#40432=CARTESIAN_POINT('Origin',(1.885,-10.2,8.9275));
#40433=CARTESIAN_POINT('',(6.13375000000003,-14.4487500000001,5.52124999999999));
#40434=CARTESIAN_POINT('Origin',(1.86,-34.9,9.795));
#40435=CARTESIAN_POINT('',(1.735,-34.9,9.92));
#40436=CARTESIAN_POINT('Origin',(-1.985,-34.9,9.92));
#40437=CARTESIAN_POINT('Origin',(-1.86,-34.9,6.075));
#40438=CARTESIAN_POINT('Origin',(0.,-34.9,7.935));
#40439=CARTESIAN_POINT('',(0.,0.,0.));
#40440=CARTESIAN_POINT('Origin',(0.,17.,0.));
#40441=CARTESIAN_POINT('',(23.5,16.,7.31881207649691E-15));
#40442=CARTESIAN_POINT('',(22.5,17.,7.07388271666744E-15));
#40443=CARTESIAN_POINT('Origin',(23.5,17.,7.31881207649691E-15));
#40444=CARTESIAN_POINT('Origin',(23.5,17.,7.31881207649691E-15));
#40445=CARTESIAN_POINT('',(-22.5,17.,-4.31842741858589E-15));
#40446=CARTESIAN_POINT('Origin',(0.,17.,0.));
#40447=CARTESIAN_POINT('',(-23.5,16.,-4.44089209850063E-15));
#40448=CARTESIAN_POINT('Origin',(-23.5,17.,-4.44089209850063E-15));
#40449=CARTESIAN_POINT('Origin',(-23.5,17.,-4.44089209850063E-15));
#40450=CARTESIAN_POINT('Origin',(-23.5,17.,-33.));
#40451=CARTESIAN_POINT('',(-23.5,16.,-33.));
#40452=CARTESIAN_POINT('',(-23.5,16.,-33.));
#40453=CARTESIAN_POINT('',(-22.5,17.,-33.));
#40454=CARTESIAN_POINT('Origin',(-23.5,17.,-33.));
#40455=CARTESIAN_POINT('Origin',(-23.5,17.,-33.));
#40456=CARTESIAN_POINT('Origin',(0.,17.,-33.));
#40457=CARTESIAN_POINT('',(22.5,17.,-33.));
#40458=CARTESIAN_POINT('Origin',(0.,17.,-33.));
#40459=CARTESIAN_POINT('',(23.5,16.,-33.));
#40460=CARTESIAN_POINT('Origin',(23.5,17.,-33.));
#40461=CARTESIAN_POINT('Origin',(23.5,17.,-33.));
#40462=CARTESIAN_POINT('Origin',(23.5,17.,-16.5));
#40463=CARTESIAN_POINT('',(23.5,16.,-16.5));
#40464=CARTESIAN_POINT('',(0.,0.,0.));
#40465=CARTESIAN_POINT('Origin',(0.,1.11022302462516E-15,-9.52627944162883));
#40466=CARTESIAN_POINT('',(0.5,-0.433012701892221,-9.85362971081845));
#40467=CARTESIAN_POINT('',(0.5,0.433012701892217,-9.85362971081845));
#40468=CARTESIAN_POINT('',(0.5,-0.433012701892222,-9.85362971081845));
#40469=CARTESIAN_POINT('',(0.,0.,-9.52627944162883));
#40470=CARTESIAN_POINT('',(0.,1.11022302462516E-15,-9.52627944162883));
#40471=CARTESIAN_POINT('',(0.5,0.433012701892217,-9.85362971081845));
#40472=CARTESIAN_POINT('Origin',(0.5,8.75,-4.55181485540923));
#40473=CARTESIAN_POINT('',(0.,8.25,-4.76313972081442));
#40474=CARTESIAN_POINT('',(0.5,8.31698729810778,-5.30181485540923));
#40475=CARTESIAN_POINT('',(0.,8.24999999999999,-4.76313972081442));
#40476=CARTESIAN_POINT('',(0.5,8.75,-4.55181485540923));
#40477=CARTESIAN_POINT('',(0.5,8.75,-4.55181485540923));
#40478=CARTESIAN_POINT('',(0.5,8.31698729810778,-5.30181485540923));
#40479=CARTESIAN_POINT('Origin',(0.,-8.25,-4.76313972081441));
#40480=CARTESIAN_POINT('',(0.5,-8.75,-4.55181485540923));
#40481=CARTESIAN_POINT('',(0.5,-8.31698729810778,-5.30181485540923));
#40482=CARTESIAN_POINT('',(0.5,-8.75,-4.55181485540923));
#40483=CARTESIAN_POINT('',(0.,-8.25,-4.76313972081441));
#40484=CARTESIAN_POINT('',(0.,-8.25,-4.76313972081441));
#40485=CARTESIAN_POINT('',(0.5,-8.31698729810778,-5.30181485540923));
#40486=CARTESIAN_POINT('Origin',(0.,8.25,4.76313972081441));
#40487=CARTESIAN_POINT('',(0.5,8.75,4.55181485540922));
#40488=CARTESIAN_POINT('',(0.5,8.31698729810778,5.30181485540922));
#40489=CARTESIAN_POINT('',(0.5,8.75,4.55181485540922));
#40490=CARTESIAN_POINT('',(0.,8.25,4.76313972081441));
#40491=CARTESIAN_POINT('',(0.,8.25,4.76313972081441));
#40492=CARTESIAN_POINT('',(0.5,8.31698729810778,5.30181485540922));
#40493=CARTESIAN_POINT('Origin',(0.25,8.5,-2.52590742770462));
#40494=CARTESIAN_POINT('',(0.5,8.75,-2.52590742770462));
#40495=CARTESIAN_POINT('',(0.,8.25,-2.52590742770462));
#40496=CARTESIAN_POINT('Origin',(0.,-8.25,4.76313972081441));
#40497=CARTESIAN_POINT('',(0.5,-8.31698729810778,5.30181485540922));
#40498=CARTESIAN_POINT('',(0.5,-8.75,4.55181485540922));
#40499=CARTESIAN_POINT('',(0.5,-8.31698729810778,5.30181485540922));
#40500=CARTESIAN_POINT('',(0.,-8.25,4.76313972081441));
#40501=CARTESIAN_POINT('',(0.,-8.25,4.76313972081441));
#40502=CARTESIAN_POINT('',(0.5,-8.75,4.55181485540922));
#40503=CARTESIAN_POINT('Origin',(0.,-1.11022302462516E-15,9.52627944162883));
#40504=CARTESIAN_POINT('',(0.5,0.433012701892218,9.85362971081845));
#40505=CARTESIAN_POINT('',(0.5,-0.433012701892219,9.85362971081845));
#40506=CARTESIAN_POINT('',(0.5,0.433012701892219,9.85362971081845));
#40507=CARTESIAN_POINT('',(0.,2.77555756156289E-16,9.52627944162883));
#40508=CARTESIAN_POINT('',(0.,-1.11022302462516E-15,9.52627944162883));
#40509=CARTESIAN_POINT('',(0.5,-0.433012701892219,9.85362971081845));
#40510=CARTESIAN_POINT('Origin',(0.25,6.4375,6.09826221831542));
#40511=CARTESIAN_POINT('',(0.5,6.5625,6.31476856926153));
#40512=CARTESIAN_POINT('',(0.,6.3125,5.88175586736931));
#40513=CARTESIAN_POINT('Origin',(0.25,-2.0625,8.62416964602003));
#40514=CARTESIAN_POINT('',(0.5,-2.1875,8.84067599696614));
#40515=CARTESIAN_POINT('',(0.,-1.9375,8.40766329507393));
#40516=CARTESIAN_POINT('Origin',(0.,0.,9.85362971081845));
#40517=CARTESIAN_POINT('',(5.19749458287263,-0.43301270189222,9.85362971081845));
#40518=CARTESIAN_POINT('',(5.19749458287263,0.433012701892219,9.85362971081845));
#40519=CARTESIAN_POINT('Ctrl Pts',(5.19749458287264,-0.43301270189222,9.85362971081845));
#40520=CARTESIAN_POINT('Ctrl Pts',(5.20847043415501,1.38777878078145E-14,
9.85362971081845));
#40521=CARTESIAN_POINT('Ctrl Pts',(5.19749458287263,0.433012701892219,9.85362971081845));
#40522=CARTESIAN_POINT('',(0.,0.433012701892219,9.85362971081845));
#40523=CARTESIAN_POINT('',(0.,-0.433012701892219,9.85362971081845));
#40524=CARTESIAN_POINT('Origin',(0.25,-8.5,2.52590742770461));
#40525=CARTESIAN_POINT('',(0.5,-8.75,2.52590742770461));
#40526=CARTESIAN_POINT('',(0.,-8.25,2.52590742770461));
#40527=CARTESIAN_POINT('Origin',(0.,-8.53349364905389,4.92681485540922));
#40528=CARTESIAN_POINT('',(5.19749458287263,-8.75,4.55181485540923));
#40529=CARTESIAN_POINT('',(5.19749458287263,-8.31698729810778,5.30181485540922));
#40530=CARTESIAN_POINT('Ctrl Pts',(5.19749458287263,-8.75,4.55181485540923));
#40531=CARTESIAN_POINT('Ctrl Pts',(5.20847043415501,-8.53349364905388,4.92681485540924));
#40532=CARTESIAN_POINT('Ctrl Pts',(5.19749458287263,-8.31698729810778,5.30181485540922));
#40533=CARTESIAN_POINT('',(0.,-8.31698729810778,5.30181485540922));
#40534=CARTESIAN_POINT('',(0.,-8.75,4.55181485540922));
#40535=CARTESIAN_POINT('Origin',(0.,8.53349364905389,4.92681485540922));
#40536=CARTESIAN_POINT('',(5.19749458287264,8.31698729810778,5.30181485540922));
#40537=CARTESIAN_POINT('',(5.19749458287263,8.75,4.55181485540922));
#40538=CARTESIAN_POINT('Ctrl Pts',(5.19749458287264,8.31698729810778,5.30181485540922));
#40539=CARTESIAN_POINT('Ctrl Pts',(5.20847043415501,8.5334936490539,4.92681485540921));
#40540=CARTESIAN_POINT('Ctrl Pts',(5.19749458287263,8.75,4.55181485540922));
#40541=CARTESIAN_POINT('',(0.,8.75,4.55181485540922));
#40542=CARTESIAN_POINT('',(0.,8.31698729810778,5.30181485540922));
#40543=CARTESIAN_POINT('Origin',(0.25,-6.4375,-6.09826221831542));
#40544=CARTESIAN_POINT('',(0.5,-6.5625,-6.31476856926153));
#40545=CARTESIAN_POINT('',(0.,-6.3125,-5.88175586736931));
#40546=CARTESIAN_POINT('Origin',(0.,-8.53349364905389,-4.92681485540923));
#40547=CARTESIAN_POINT('',(5.19749458287263,-8.31698729810778,-5.30181485540923));
#40548=CARTESIAN_POINT('',(5.19749458287263,-8.75,-4.55181485540923));
#40549=CARTESIAN_POINT('Ctrl Pts',(5.19749458287263,-8.31698729810778,-5.30181485540923));
#40550=CARTESIAN_POINT('Ctrl Pts',(5.20847043415501,-8.5334936490539,-4.92681485540921));
#40551=CARTESIAN_POINT('Ctrl Pts',(5.19749458287263,-8.75,-4.55181485540923));
#40552=CARTESIAN_POINT('',(0.,-8.75,-4.55181485540923));
#40553=CARTESIAN_POINT('',(0.,-8.31698729810778,-5.30181485540923));
#40554=CARTESIAN_POINT('Origin',(0.,8.53349364905389,-4.92681485540923));
#40555=CARTESIAN_POINT('',(5.19749458287263,8.75,-4.55181485540923));
#40556=CARTESIAN_POINT('',(5.19749458287263,8.31698729810778,-5.30181485540923));
#40557=CARTESIAN_POINT('Ctrl Pts',(5.19749458287263,8.75,-4.55181485540923));
#40558=CARTESIAN_POINT('Ctrl Pts',(5.20847043415501,8.53349364905388,-4.92681485540924));
#40559=CARTESIAN_POINT('Ctrl Pts',(5.19749458287263,8.31698729810778,-5.30181485540923));
#40560=CARTESIAN_POINT('',(0.,8.31698729810778,-5.30181485540923));
#40561=CARTESIAN_POINT('',(0.,8.75,-4.55181485540923));
#40562=CARTESIAN_POINT('Origin',(0.25,2.0625,-8.62416964602004));
#40563=CARTESIAN_POINT('',(0.5,2.1875,-8.84067599696614));
#40564=CARTESIAN_POINT('',(0.,1.9375,-8.40766329507393));
#40565=CARTESIAN_POINT('Origin',(0.,-2.42861286636753E-15,-9.85362971081845));
#40566=CARTESIAN_POINT('',(5.19749458287263,0.433012701892218,-9.85362971081845));
#40567=CARTESIAN_POINT('',(5.19749458287263,-0.433012701892222,-9.85362971081845));
#40568=CARTESIAN_POINT('Ctrl Pts',(5.19749458287263,0.433012701892218,-9.85362971081845));
#40569=CARTESIAN_POINT('Ctrl Pts',(5.20847043415501,-1.65145674912992E-14,
-9.85362971081845));
#40570=CARTESIAN_POINT('Ctrl Pts',(5.19749458287263,-0.433012701892222,
-9.85362971081845));
#40571=CARTESIAN_POINT('',(0.,-0.433012701892222,-9.85362971081845));
#40572=CARTESIAN_POINT('',(0.,0.433012701892217,-9.85362971081845));
#40573=CARTESIAN_POINT('Origin',(0.,6.18668889256196E-16,10.1036297108185));
#40574=CARTESIAN_POINT('Ctrl Pts',(5.19749458287263,-8.31698729810778,5.30181485540922));
#40575=CARTESIAN_POINT('Ctrl Pts',(6.41034186570176,-4.375,7.57772228311384));
#40576=CARTESIAN_POINT('Ctrl Pts',(5.19749458287263,-0.43301270189222,9.85362971081845));
#40577=CARTESIAN_POINT('Origin',(0.,-8.75,5.05181485540922));
#40578=CARTESIAN_POINT('',(5.84018475750577,-8.75,-1.10351065767392E-15));
#40579=CARTESIAN_POINT('Ctrl Pts',(5.19749458287264,-8.75,-4.55181485540923));
#40580=CARTESIAN_POINT('Ctrl Pts',(5.84018475750577,-8.75,-2.13979915834902));
#40581=CARTESIAN_POINT('Ctrl Pts',(5.84018475750577,-8.75,-1.13545536609391E-15));
#40582=CARTESIAN_POINT('Ctrl Pts',(5.84018475750577,-8.75,-1.13545536609391E-15));
#40583=CARTESIAN_POINT('Ctrl Pts',(5.84018475750577,-8.75,2.13979915834902));
#40584=CARTESIAN_POINT('Ctrl Pts',(5.19749458287263,-8.75,4.55181485540923));
#40585=CARTESIAN_POINT('Origin',(0.,-8.75,-5.05181485540923));
#40586=CARTESIAN_POINT('Ctrl Pts',(5.19749458287263,-0.433012701892222,
-9.85362971081845));
#40587=CARTESIAN_POINT('Ctrl Pts',(6.41034186570176,-4.375,-7.57772228311384));
#40588=CARTESIAN_POINT('Ctrl Pts',(5.19749458287263,-8.31698729810778,-5.30181485540923));
#40589=CARTESIAN_POINT('Origin',(0.,0.,0.));
#40590=CARTESIAN_POINT('',(1.38777878078145E-16,-6.2,-7.59281015471359E-16));
#40591=CARTESIAN_POINT('Origin',(0.,0.,0.));
#40592=CARTESIAN_POINT('Origin',(5.75,-0.875,-3.24759526419165));
#40593=CARTESIAN_POINT('',(6.,-3.5,-2.02072594216369));
#40594=CARTESIAN_POINT('',(6.,-5.55111512312578E-16,-4.04145188432738));
#40595=CARTESIAN_POINT('',(6.,-1.,-3.46410161513775));
#40596=CARTESIAN_POINT('',(5.5,-6.36345143234944E-16,-3.46410161513775));
#40597=CARTESIAN_POINT('',(6.,-2.77555756156289E-16,-4.04145188432738));
#40598=CARTESIAN_POINT('',(5.5,-3.,-1.73205080756888));
#40599=CARTESIAN_POINT('',(5.5,-0.75,-3.03108891324554));
#40600=CARTESIAN_POINT('',(6.,-3.5,-2.02072594216369));
#40601=CARTESIAN_POINT('Origin',(5.75,2.375,-2.38156986040721));
#40602=CARTESIAN_POINT('',(6.,3.5,-2.02072594216369));
#40603=CARTESIAN_POINT('',(6.,2.5,-2.59807621135332));
#40604=CARTESIAN_POINT('',(5.5,3.,-1.73205080756888));
#40605=CARTESIAN_POINT('',(6.,3.5,-2.02072594216369));
#40606=CARTESIAN_POINT('',(5.5,2.25,-2.1650635094611));
#40607=CARTESIAN_POINT('Origin',(5.75,0.875,3.24759526419165));
#40608=CARTESIAN_POINT('',(6.,3.5,2.02072594216369));
#40609=CARTESIAN_POINT('',(6.,-5.55111512312578E-16,4.04145188432738));
#40610=CARTESIAN_POINT('',(6.,1.,3.46410161513775));
#40611=CARTESIAN_POINT('',(5.5,2.12115047744981E-16,3.46410161513775));
#40612=CARTESIAN_POINT('',(6.,-5.55111512312578E-16,4.04145188432738));
#40613=CARTESIAN_POINT('',(5.5,3.,1.73205080756888));
#40614=CARTESIAN_POINT('',(5.5,0.75,3.03108891324554));
#40615=CARTESIAN_POINT('',(5.5,3.,1.73205080756888));
#40616=CARTESIAN_POINT('Origin',(5.75,-2.375,2.38156986040721));
#40617=CARTESIAN_POINT('',(5.5,-3.,1.73205080756888));
#40618=CARTESIAN_POINT('',(5.5,-2.25,2.1650635094611));
#40619=CARTESIAN_POINT('',(6.,-3.5,2.02072594216369));
#40620=CARTESIAN_POINT('',(6.,-2.5,2.59807621135332));
#40621=CARTESIAN_POINT('',(6.,-3.5,2.02072594216369));
#40622=CARTESIAN_POINT('Origin',(5.75,3.25,0.866025403784438));
#40623=CARTESIAN_POINT('',(6.,3.5,0.866025403784438));
#40624=CARTESIAN_POINT('',(5.5,3.,0.866025403784438));
#40625=CARTESIAN_POINT('Origin',(5.75,-3.25,-0.866025403784439));
#40626=CARTESIAN_POINT('',(5.5,-3.,-0.866025403784439));
#40627=CARTESIAN_POINT('',(6.,-3.5,-0.866025403784439));
#40628=CARTESIAN_POINT('Origin',(6.,3.,-1.73205080756888));
#40629=CARTESIAN_POINT('',(2.,3.,-1.73205080756888));
#40630=CARTESIAN_POINT('',(6.,3.,-1.73205080756888));
#40631=CARTESIAN_POINT('',(2.,-5.55111512312578E-16,-3.46410161513775));
#40632=CARTESIAN_POINT('',(2.,-6.36345143234944E-16,-3.46410161513775));
#40633=CARTESIAN_POINT('',(6.,-6.36345143234944E-16,-3.46410161513775));
#40634=CARTESIAN_POINT('Origin',(6.,3.,1.73205080756888));
#40635=CARTESIAN_POINT('',(2.,3.,1.73205080756888));
#40636=CARTESIAN_POINT('',(6.,3.,1.73205080756888));
#40637=CARTESIAN_POINT('',(2.,3.,-1.73205080756888));
#40638=CARTESIAN_POINT('Origin',(6.,0.,3.46410161513775));
#40639=CARTESIAN_POINT('',(2.,0.,3.46410161513775));
#40640=CARTESIAN_POINT('',(6.,2.12115047744981E-16,3.46410161513775));
#40641=CARTESIAN_POINT('',(2.,3.,1.73205080756888));
#40642=CARTESIAN_POINT('Origin',(6.,0.,0.));
#40643=CARTESIAN_POINT('',(6.,-8.4732,-1.03766772585354E-15));
#40644=CARTESIAN_POINT('Origin',(6.,0.,0.));
#40645=CARTESIAN_POINT('Origin',(6.,-3.,1.73205080756888));
#40646=CARTESIAN_POINT('',(2.,-3.,1.73205080756888));
#40647=CARTESIAN_POINT('',(6.,-3.,1.73205080756888));
#40648=CARTESIAN_POINT('',(2.,2.12115047744981E-16,3.46410161513775));
#40649=CARTESIAN_POINT('Origin',(6.,-3.,-1.73205080756888));
#40650=CARTESIAN_POINT('',(2.,-3.,-1.73205080756888));
#40651=CARTESIAN_POINT('',(6.,-3.,-1.73205080756888));
#40652=CARTESIAN_POINT('',(2.,-3.,1.73205080756888));
#40653=CARTESIAN_POINT('Origin',(6.,-5.55111512312578E-16,-3.46410161513775));
#40654=CARTESIAN_POINT('',(2.,-3.,-1.73205080756888));
#40655=CARTESIAN_POINT('Origin',(2.,0.,0.));
#40656=CARTESIAN_POINT('Origin',(5.464896073903,0.,0.));
#40657=CARTESIAN_POINT('',(5.464896073903,-9.4,-1.15116799119851E-15));
#40658=CARTESIAN_POINT('Ctrl Pts',(5.19749458287263,8.31698729810778,-5.30181485540923));
#40659=CARTESIAN_POINT('Ctrl Pts',(6.41034186570176,4.375,-7.57772228311383));
#40660=CARTESIAN_POINT('Ctrl Pts',(5.19749458287263,0.43301270189222,-9.85362971081845));
#40661=CARTESIAN_POINT('Ctrl Pts',(5.19749458287263,8.75,4.55181485540922));
#40662=CARTESIAN_POINT('Ctrl Pts',(6.41034186570176,8.75,-6.10622663543836E-15));
#40663=CARTESIAN_POINT('Ctrl Pts',(5.19749458287263,8.75,-4.55181485540923));
#40664=CARTESIAN_POINT('Ctrl Pts',(5.19749458287263,0.433012701892218,9.85362971081845));
#40665=CARTESIAN_POINT('Ctrl Pts',(6.41034186570176,4.375,7.57772228311384));
#40666=CARTESIAN_POINT('Ctrl Pts',(5.19749458287264,8.31698729810778,5.30181485540922));
#40667=CARTESIAN_POINT('Origin',(0.,8.75,5.05181485540922));
#40668=CARTESIAN_POINT('Origin',(0.,8.75,-5.05181485540923));
#40669=CARTESIAN_POINT('Origin',(0.,-1.85600666776859E-15,-10.1036297108185));
#40670=CARTESIAN_POINT('Origin',(-11.,6.64,0.));
#40671=CARTESIAN_POINT('',(-11.,-6.64,-8.13165474633843E-16));
#40672=CARTESIAN_POINT('Origin',(-11.,0.,0.));
#40673=CARTESIAN_POINT('Origin',(-10.75,0.,0.));
#40674=CARTESIAN_POINT('',(-10.5,-7.14,-8.7439781459121E-16));
#40675=CARTESIAN_POINT('Origin',(-10.5,0.,0.));
#40676=CARTESIAN_POINT('',(-10.75,-6.89,-8.43781644612526E-16));
#40677=CARTESIAN_POINT('Origin',(-6.25,0.,0.));
#40678=CARTESIAN_POINT('',(-2.,-7.14,-8.7439781459121E-16));
#40679=CARTESIAN_POINT('Origin',(-2.,0.,0.));
#40680=CARTESIAN_POINT('',(-6.25,-7.14,-8.7439781459121E-16));
#40681=CARTESIAN_POINT('Origin',(-2.,6.2,0.));
#40682=CARTESIAN_POINT('',(-2.,-6.2,-7.59281015471359E-16));
#40683=CARTESIAN_POINT('Origin',(-2.,0.,0.));
#40684=CARTESIAN_POINT('Origin',(-1.,0.,0.));
#40685=CARTESIAN_POINT('',(-1.,-6.2,-7.59281015471359E-16));
#40686=CARTESIAN_POINT('',(0.,0.,0.));
#40687=CARTESIAN_POINT('Origin',(8.,0.,0.));
#40688=CARTESIAN_POINT('',(14.8,-8.5,-1.04094977927525E-15));
#40689=CARTESIAN_POINT('Origin',(14.8,0.,0.));
#40690=CARTESIAN_POINT('',(1.2,-8.5,-1.04094977927525E-15));
#40691=CARTESIAN_POINT('',(8.,-8.5,-1.04094977927525E-15));
#40692=CARTESIAN_POINT('Origin',(1.2,0.,0.));
#40693=CARTESIAN_POINT('Origin',(1.2,10.7,0.));
#40694=CARTESIAN_POINT('',(1.2,-10.7,-1.31037207508767E-15));
#40695=CARTESIAN_POINT('Origin',(1.2,0.,0.));
#40696=CARTESIAN_POINT('Origin',(14.8,8.5,0.));
#40697=CARTESIAN_POINT('',(14.8,-10.7,-1.31037207508767E-15));
#40698=CARTESIAN_POINT('Origin',(14.8,0.,0.));
#40699=CARTESIAN_POINT('Origin',(8.,0.,0.));
#40700=CARTESIAN_POINT('',(15.3,-10.7,-1.31037207508767E-15));
#40701=CARTESIAN_POINT('Origin',(15.3,0.,0.));
#40702=CARTESIAN_POINT('',(8.,-10.7,-1.31037207508767E-15));
#40703=CARTESIAN_POINT('Origin',(0.35,0.,0.));
#40704=CARTESIAN_POINT('',(0.7,-9.,-1.10218211923262E-15));
#40705=CARTESIAN_POINT('Origin',(0.7,0.,0.));
#40706=CARTESIAN_POINT('',(0.,-9.,-1.10218211923262E-15));
#40707=CARTESIAN_POINT('',(0.35,-9.,-1.10218211923262E-15));
#40708=CARTESIAN_POINT('Origin',(0.,0.,0.));
#40709=CARTESIAN_POINT('Origin',(0.,11.5,0.));
#40710=CARTESIAN_POINT('',(0.,-11.5,-1.40834381901946E-15));
#40711=CARTESIAN_POINT('Origin',(0.,0.,0.));
#40712=CARTESIAN_POINT('Origin',(8.,0.,0.));
#40713=CARTESIAN_POINT('',(16.,-11.5,-1.40834381901946E-15));
#40714=CARTESIAN_POINT('Origin',(16.,0.,0.));
#40715=CARTESIAN_POINT('',(8.,-11.5,-1.40834381901946E-15));
#40716=CARTESIAN_POINT('Origin',(16.,9.,0.));
#40717=CARTESIAN_POINT('',(16.,-9.,-1.10218211923262E-15));
#40718=CARTESIAN_POINT('Origin',(16.,0.,0.));
#40719=CARTESIAN_POINT('Origin',(15.65,0.,0.));
#40720=CARTESIAN_POINT('',(15.3,-9.,-1.10218211923262E-15));
#40721=CARTESIAN_POINT('',(15.65,-9.,-1.10218211923262E-15));
#40722=CARTESIAN_POINT('Origin',(15.3,0.,0.));
#40723=CARTESIAN_POINT('Origin',(15.3,10.7,0.));
#40724=CARTESIAN_POINT('Origin',(8.,0.,0.));
#40725=CARTESIAN_POINT('',(0.7,-10.7,-1.31037207508767E-15));
#40726=CARTESIAN_POINT('',(8.,-10.7,-1.31037207508767E-15));
#40727=CARTESIAN_POINT('Origin',(0.7,0.,0.));
#40728=CARTESIAN_POINT('Origin',(0.7,9.,0.));
#40729=CARTESIAN_POINT('',(0.,0.,0.));
#40730=CARTESIAN_POINT('Origin',(-74.75,0.,0.));
#40731=CARTESIAN_POINT('',(-89.0911584740964,-4.92496730081785,0.000125565713578885));
#40732=CARTESIAN_POINT('',(-89.3088415259036,-4.92497224643154,8.66411886420825E-5));
#40733=CARTESIAN_POINT('',(-74.75,-4.925,-6.03138548580071E-16));
#40734=CARTESIAN_POINT('',(-89.575,2.16848376312314,4.42201352087158));
#40735=CARTESIAN_POINT('Ctrl Pts',(-89.0911584740964,-4.92496730081785,
0.000125565713578885));
#40736=CARTESIAN_POINT('Ctrl Pts',(-89.1008019864049,-4.92516638575022,
0.199069300706784));
#40737=CARTESIAN_POINT('Ctrl Pts',(-89.1104454987134,-4.91333770780035,
0.39798946055041));
#40738=CARTESIAN_POINT('Ctrl Pts',(-89.1200890110219,-4.889294230975,0.595422009497546));
#40739=CARTESIAN_POINT('Ctrl Pts',(-89.1595997107719,-4.79078504019411,
1.40432834080175));
#40740=CARTESIAN_POINT('Ctrl Pts',(-89.1991104105219,-4.48723269016115,
2.18826296024533));
#40741=CARTESIAN_POINT('Ctrl Pts',(-89.2386211102719,-4.01529023278917,
2.85257156086601));
#40742=CARTESIAN_POINT('Ctrl Pts',(-89.278131810022,-3.5433477754172,3.51688016148669));
#40743=CARTESIAN_POINT('Ctrl Pts',(-89.317642509772,-2.90301521070621,4.06156274328447));
#40744=CARTESIAN_POINT('Ctrl Pts',(-89.357153209522,-2.17161165738311,4.42084202425627));
#40745=CARTESIAN_POINT('Ctrl Pts',(-89.396663909272,-1.44020810406001,4.78012130522807));
#40746=CARTESIAN_POINT('Ctrl Pts',(-89.4361746090221,-0.617733562124788,
4.95399728537389));
#40747=CARTESIAN_POINT('Ctrl Pts',(-89.4756853087721,0.196500867390113,
4.92149114064075));
#40748=CARTESIAN_POINT('Ctrl Pts',(-89.5087902058481,0.878724851154841,
4.89425516196826));
#40749=CARTESIAN_POINT('Ctrl Pts',(-89.5418951029241,1.55516403718748,4.72213295031185));
#40750=CARTESIAN_POINT('Ctrl Pts',(-89.575,2.16857165393607,4.42207223182617));
#40751=CARTESIAN_POINT('',(-89.575,-2.16839587231079,4.42195480991671));
#40752=CARTESIAN_POINT('Origin',(-89.575,0.,0.));
#40753=CARTESIAN_POINT('Ctrl Pts',(-89.575,-2.16839587231078,4.42195480991671));
#40754=CARTESIAN_POINT('Ctrl Pts',(-89.53548930025,-2.90023837919386,4.06308088665816));
#40755=CARTESIAN_POINT('Ctrl Pts',(-89.4959786004999,-3.54091307931629,
3.5192055949212));
#40756=CARTESIAN_POINT('Ctrl Pts',(-89.4564679007499,-4.01330868267018,
2.85533993012661));
#40757=CARTESIAN_POINT('Ctrl Pts',(-89.4169572009999,-4.48570428602409,
2.191474265332));
#40758=CARTESIAN_POINT('Ctrl Pts',(-89.3774465012498,-4.78982079260945,
1.40761822747977));
#40759=CARTESIAN_POINT('Ctrl Pts',(-89.3379358014998,-4.88889138955698,
0.598745942138952));
#40760=CARTESIAN_POINT('Ctrl Pts',(-89.3282377096344,-4.91320874552475,
0.400204337453629));
#40761=CARTESIAN_POINT('Ctrl Pts',(-89.318539617769,-4.92517248101639,0.200155552119072));
#40762=CARTESIAN_POINT('Ctrl Pts',(-89.3088415259036,-4.92497224643154,
8.66411886420825E-5));
#40763=CARTESIAN_POINT('Origin',(-74.75,0.,0.));
#40764=CARTESIAN_POINT('',(-87.5911584740964,-4.92530808678391,-7.85116754067894E-5));
#40765=CARTESIAN_POINT('',(-87.8088415259036,-4.92531071258075,-7.76212487999366E-5));
#40766=CARTESIAN_POINT('',(-74.75,-4.925,-6.03138548580071E-16));
#40767=CARTESIAN_POINT('Ctrl Pts',(-87.5911584740964,-4.92530808678391,
-7.85116754067894E-5));
#40768=CARTESIAN_POINT('Ctrl Pts',(-87.6266735894045,-4.9247489168746,0.732444837198349));
#40769=CARTESIAN_POINT('Ctrl Pts',(-87.6621887047127,-4.75913849024366,
1.46521259091458));
#40770=CARTESIAN_POINT('Ctrl Pts',(-87.6977038200208,-4.44298152154857,
2.1259445723498));
#40771=CARTESIAN_POINT('Ctrl Pts',(-87.7372145197708,-4.09125570127135,
2.8610113941026));
#40772=CARTESIAN_POINT('Ctrl Pts',(-87.7767252195208,-3.55320374873502,
3.50692208746224));
#40773=CARTESIAN_POINT('Ctrl Pts',(-87.8162359192709,-2.89379421649954,
3.98568440246682));
#40774=CARTESIAN_POINT('Ctrl Pts',(-87.8557466190209,-2.23438468426406,
4.46444671747141));
#40775=CARTESIAN_POINT('Ctrl Pts',(-87.895257318771,-1.45361757232942,4.77606065412094));
#40776=CARTESIAN_POINT('Ctrl Pts',(-87.934768018521,-0.645768738251389,
4.88289953469631));
#40777=CARTESIAN_POINT('Ctrl Pts',(-87.974278718271,0.162080095826638,4.98973841527168));
#40778=CARTESIAN_POINT('Ctrl Pts',(-88.013789418021,0.997010652048049,4.89180223977289));
#40779=CARTESIAN_POINT('Ctrl Pts',(-88.053300117771,1.75820696011884,4.60091658286799));
#40780=CARTESIAN_POINT('Ctrl Pts',(-88.0928108175211,2.51940326818962,4.3100309259631));
#40781=CARTESIAN_POINT('Ctrl Pts',(-88.1323215172712,3.20686532810979,3.8261957876521));
#40782=CARTESIAN_POINT('Ctrl Pts',(-88.1718322170212,3.73758365539158,3.20783315584934));
#40783=CARTESIAN_POINT('Ctrl Pts',(-88.2113429167712,4.26830198267335,2.58947052404659));
#40784=CARTESIAN_POINT('Ctrl Pts',(-88.2508536165212,4.64227657731676,1.83658039875207));
#40785=CARTESIAN_POINT('Ctrl Pts',(-88.2903643162712,4.81435085620369,1.04007256938689));
#40786=CARTESIAN_POINT('Ctrl Pts',(-88.3298750160212,4.98642513509063,0.243564740021695));
#40787=CARTESIAN_POINT('Ctrl Pts',(-88.3693857157714,4.9565990982211,-0.596560793414167));
#40788=CARTESIAN_POINT('Ctrl Pts',(-88.4088964155214,4.72847417035112,-1.37886080863689));
#40789=CARTESIAN_POINT('Ctrl Pts',(-88.4484071152714,4.50034924248114,-2.16116082385961));
#40790=CARTESIAN_POINT('Ctrl Pts',(-88.4879178150213,4.07392542361072,-2.88563532086918));
#40791=CARTESIAN_POINT('Ctrl Pts',(-88.5274285147714,3.50069242553572,-3.46480558750653));
#40792=CARTESIAN_POINT('Ctrl Pts',(-88.5669392145214,2.92745942746073,-4.04397585414388));
#40793=CARTESIAN_POINT('Ctrl Pts',(-88.6064499142716,2.20741725018117,-4.47784189040901));
#40794=CARTESIAN_POINT('Ctrl Pts',(-88.6459606140216,1.42750934685709,-4.71401547804238));
#40795=CARTESIAN_POINT('Ctrl Pts',(-88.6854713137716,0.647601443533018,
-4.95018906567576));
#40796=CARTESIAN_POINT('Ctrl Pts',(-88.7249820135216,-0.192172185835564,
-4.98867020467737));
#40797=CARTESIAN_POINT('Ctrl Pts',(-88.7644927132716,-0.990410768169421,
-4.82481214047709));
#40798=CARTESIAN_POINT('Ctrl Pts',(-88.8040034130216,-1.78864935050328,
-4.6609540762768));
#40799=CARTESIAN_POINT('Ctrl Pts',(-88.8435141127716,-2.54535288580243,
-4.2947568088746));
#40800=CARTESIAN_POINT('Ctrl Pts',(-88.8830248125217,-3.16915116407065,
-3.77043831961749));
#40801=CARTESIAN_POINT('Ctrl Pts',(-88.9225355122717,-3.79294944233888,
-3.24611983036038));
#40802=CARTESIAN_POINT('Ctrl Pts',(-88.9620462120217,-4.2838424635762,-2.56368011924835));
#40803=CARTESIAN_POINT('Ctrl Pts',(-89.0015569117718,-4.58255595843045,
-1.80552124210991));
#40804=CARTESIAN_POINT('Ctrl Pts',(-89.0314240992133,-4.80836142374944,
-1.23240880833286));
#40805=CARTESIAN_POINT('Ctrl Pts',(-89.0612912866549,-4.92435070939332,
-0.616028552547382));
#40806=CARTESIAN_POINT('Ctrl Pts',(-89.0911584740964,-4.92496730081785,
0.000125565713578885));
#40807=CARTESIAN_POINT('Ctrl Pts',(-89.3088415259036,-4.92497224643154,
8.66411886420825E-5));
#40808=CARTESIAN_POINT('Ctrl Pts',(-89.279028918019,-4.92435671141227,-0.614939084929097));
#40809=CARTESIAN_POINT('Ctrl Pts',(-89.2492163101344,-4.80879283960139,
-1.23015499597478));
#40810=CARTESIAN_POINT('Ctrl Pts',(-89.2194037022498,-4.58378991023707,
-1.80236265130469));
#40811=CARTESIAN_POINT('Ctrl Pts',(-89.1798930024997,-4.28559314665994,
-2.56071042657812));
#40812=CARTESIAN_POINT('Ctrl Pts',(-89.1403823027497,-3.79517493219598,
-3.2435174442956));
#40813=CARTESIAN_POINT('Ctrl Pts',(-89.1008716029996,-3.17173808087882,
-3.76827140867339));
#40814=CARTESIAN_POINT('Ctrl Pts',(-89.0613609032496,-2.54830122956167,
-4.29302537305117));
#40815=CARTESIAN_POINT('Ctrl Pts',(-89.0218502034996,-1.79184574139134,
-4.65972628408927));
#40816=CARTESIAN_POINT('Ctrl Pts',(-88.9823395037496,-0.993718901765311,
-4.82412795080569));
#40817=CARTESIAN_POINT('Ctrl Pts',(-88.9428288039996,-0.195592062139286,
-4.98852961752212));
#40818=CARTESIAN_POINT('Ctrl Pts',(-88.9033181042495,0.644206128942427,
-4.95063203991687));
#40819=CARTESIAN_POINT('Ctrl Pts',(-88.8638074044994,1.42427542185869,-4.71499532883177));
#40820=CARTESIAN_POINT('Ctrl Pts',(-88.8242967047494,2.20434471477496,-4.47935861774667));
#40821=CARTESIAN_POINT('Ctrl Pts',(-88.7847860049995,2.92468510952578,-4.04598277318171));
#40822=CARTESIAN_POINT('Ctrl Pts',(-88.7452753052494,3.49831541151597,-3.46720485621925));
#40823=CARTESIAN_POINT('Ctrl Pts',(-88.7057646054994,4.07194571350615,-2.88842693925679));
#40824=CARTESIAN_POINT('Ctrl Pts',(-88.6662539057493,4.49886592273571,-2.16424694989684));
#40825=CARTESIAN_POINT('Ctrl Pts',(-88.6267432059993,4.72752724946008,-1.38210405139087));
#40826=CARTESIAN_POINT('Ctrl Pts',(-88.5872325062492,4.95618857618444,-0.599961152884894));
#40827=CARTESIAN_POINT('Ctrl Pts',(-88.5477218064993,4.98659102040361,0.240144654767101));
#40828=CARTESIAN_POINT('Ctrl Pts',(-88.5082111067493,4.81506313048895,1.0367705513221));
#40829=CARTESIAN_POINT('Ctrl Pts',(-88.4687004069992,4.64353524057429,1.8333964478771));
#40830=CARTESIAN_POINT('Ctrl Pts',(-88.4291897072492,4.2700770165258,2.58654243333511));
#40831=CARTESIAN_POINT('Ctrl Pts',(-88.3896790074991,3.73978290287187,3.20526880665016));
#40832=CARTESIAN_POINT('Ctrl Pts',(-88.3501683077491,3.20948878921794,3.82399517996522));
#40833=CARTESIAN_POINT('Ctrl Pts',(-88.3106576079991,2.52235878595858,4.30830194113731));
#40834=CARTESIAN_POINT('Ctrl Pts',(-88.2711469082491,1.76136217724779,4.59970966687813));
#40835=CARTESIAN_POINT('Ctrl Pts',(-88.231636208499,1.000365568537,4.89111739261894));
#40836=CARTESIAN_POINT('Ctrl Pts',(-88.192125508749,0.165502354374793,4.98962608292848));
#40837=CARTESIAN_POINT('Ctrl Pts',(-88.1526148089989,-0.642419574094824,
4.8833412755425));
#40838=CARTESIAN_POINT('Ctrl Pts',(-88.1131041092489,-1.45034150256444,
4.77705646815652));
#40839=CARTESIAN_POINT('Ctrl Pts',(-88.0735934094989,-2.23132214534146,
4.46597816307502));
#40840=CARTESIAN_POINT('Ctrl Pts',(-88.0340827097488,-2.89105988744621,
3.98766824144186));
#40841=CARTESIAN_POINT('Ctrl Pts',(-87.9945720099988,-3.55079762955095,
3.50935831980869));
#40842=CARTESIAN_POINT('Ctrl Pts',(-87.9550613102488,-4.08929247098342,
2.86381678162386));
#40843=CARTESIAN_POINT('Ctrl Pts',(-87.9155506104988,-4.44152236847542,
2.12899136191391));
#40844=CARTESIAN_POINT('Ctrl Pts',(-87.8799809156337,-4.75861900446021,
1.46746129224844));
#40845=CARTESIAN_POINT('Ctrl Pts',(-87.8444112207687,-4.92475561418818,
0.733570332690291));
#40846=CARTESIAN_POINT('Ctrl Pts',(-87.8088415259036,-4.92531071258075,
-7.76212487999366E-5));
#40847=CARTESIAN_POINT('Origin',(-74.75,0.,0.));
#40848=CARTESIAN_POINT('',(-86.0911584740964,-4.92460688967043,-3.93952561872357E-5));
#40849=CARTESIAN_POINT('',(-86.3088415259036,-4.92460788888033,-4.03740411281871E-5));
#40850=CARTESIAN_POINT('',(-74.75,-4.925,-6.03138548580071E-16));
#40851=CARTESIAN_POINT('Ctrl Pts',(-86.0911584740964,-4.92460688967043,
-3.93952561872357E-5));
#40852=CARTESIAN_POINT('Ctrl Pts',(-86.1130344926542,-4.92447945269054,
0.451353233852372));
#40853=CARTESIAN_POINT('Ctrl Pts',(-86.1349105112119,-4.86294930864971,
0.902779916062517));
#40854=CARTESIAN_POINT('Ctrl Pts',(-86.1567865297696,-4.7404755378458,1.33701787580212));
#40855=CARTESIAN_POINT('Ctrl Pts',(-86.1962972295197,-4.5192732942697,2.12130344413084));
#40856=CARTESIAN_POINT('Ctrl Pts',(-86.2358079292698,-4.0992688572054,2.84951824818281));
#40857=CARTESIAN_POINT('Ctrl Pts',(-86.2753186290198,-3.53117680957672,
3.43373200244815));
#40858=CARTESIAN_POINT('Ctrl Pts',(-86.3148293287698,-2.96308476194804,
4.01794575671349));
#40859=CARTESIAN_POINT('Ctrl Pts',(-86.3543400285198,-2.24690510375498,
4.4581584611922));
#40860=CARTESIAN_POINT('Ctrl Pts',(-86.3938507282698,-1.46911490394863,
4.70121543051628));
#40861=CARTESIAN_POINT('Ctrl Pts',(-86.4333614280199,-0.691324704142275,
4.94427239984037));
#40862=CARTESIAN_POINT('Ctrl Pts',(-86.4728721277699,0.148076037277391,
4.99017363400982));
#40863=CARTESIAN_POINT('Ctrl Pts',(-86.51238282752,0.947731585107635,4.83337666313305));
#40864=CARTESIAN_POINT('Ctrl Pts',(-86.55189352727,1.74738713293789,4.67657969225627));
#40865=CARTESIAN_POINT('Ctrl Pts',(-86.59140422702,2.50729748717871,4.31708451633328));
#40866=CARTESIAN_POINT('Ctrl Pts',(-86.63091492677,3.13570519654186,3.79829936228145));
#40867=CARTESIAN_POINT('Ctrl Pts',(-86.67042562652,3.76411290590501,3.27951420822963));
#40868=CARTESIAN_POINT('Ctrl Pts',(-86.7099363262701,4.26101797039046,2.60143907604898));
#40869=CARTESIAN_POINT('Ctrl Pts',(-86.7494470260201,4.5664202307754,1.84594999961959));
#40870=CARTESIAN_POINT('Ctrl Pts',(-86.7889577257702,4.87182249116034,1.09046092319019));
#40871=CARTESIAN_POINT('Ctrl Pts',(-86.8284684255202,4.98572194744478,0.257557902512059));
#40872=CARTESIAN_POINT('Ctrl Pts',(-86.8679791252702,4.89436549868289,-0.552187912247182));
#40873=CARTESIAN_POINT('Ctrl Pts',(-86.9074898250202,4.803009049921,-1.36193372700643));
#40874=CARTESIAN_POINT('Ctrl Pts',(-86.9470005247703,4.50639669611276,-2.14852233584678));
#40875=CARTESIAN_POINT('Ctrl Pts',(-86.9865112245203,4.04034370606447,-2.81697494876789));
#40876=CARTESIAN_POINT('Ctrl Pts',(-87.0260219242703,3.57429071601619,-3.485427561689));
#40877=CARTESIAN_POINT('Ctrl Pts',(-87.0655326240203,2.93879708972785,-4.03574417869087));
#40878=CARTESIAN_POINT('Ctrl Pts',(-87.1050433237703,2.21059724084878,-4.40147531674411));
#40879=CARTESIAN_POINT('Ctrl Pts',(-87.1445540235204,1.48239739196973,-4.76720645479734));
#40880=CARTESIAN_POINT('Ctrl Pts',(-87.1840647232705,0.661491320499941,
-4.94835211390195));
#40881=CARTESIAN_POINT('Ctrl Pts',(-87.2235754230205,-0.152998427797419,
-4.9230393667081));
#40882=CARTESIAN_POINT('Ctrl Pts',(-87.2630861227705,-0.967488176094782,
-4.89772661951426));
#40883=CARTESIAN_POINT('Ctrl Pts',(-87.3025968225205,-1.77556160121972,
-4.66595546602198));
#40884=CARTESIAN_POINT('Ctrl Pts',(-87.3421075222705,-2.47964567033799,
-4.25571174714818));
#40885=CARTESIAN_POINT('Ctrl Pts',(-87.3816182220206,-3.18372973945627,
-3.84546802827438));
#40886=CARTESIAN_POINT('Ctrl Pts',(-87.4211289217706,-3.78382445256787,
-3.25675174401907));
#40887=CARTESIAN_POINT('Ctrl Pts',(-87.4606396215206,-4.20746973448743,
-2.56064905021327));
#40888=CARTESIAN_POINT('Ctrl Pts',(-87.5001503212707,-4.63111501640699,
-1.86454635640747));
#40889=CARTESIAN_POINT('Ctrl Pts',(-87.5396610210207,-4.87831086713451,
-1.06105725305119));
#40890=CARTESIAN_POINT('Ctrl Pts',(-87.5791717207707,-4.91920894848921,
-0.247201226300066));
#40891=CARTESIAN_POINT('Ctrl Pts',(-87.5831673052126,-4.92334483417583,
-0.164898698149252));
#40892=CARTESIAN_POINT('Ctrl Pts',(-87.5871628896545,-4.92537099550801,
-0.0824901516404431));
#40893=CARTESIAN_POINT('Ctrl Pts',(-87.5911584740964,-4.92530808678391,
-7.85116754067894E-5));
#40894=CARTESIAN_POINT('Ctrl Pts',(-87.8088415259036,-4.92531071258075,
-7.76212487999366E-5));
#40895=CARTESIAN_POINT('Ctrl Pts',(-87.8049005210186,-4.92537221565197,
-0.0813633950316671));
#40896=CARTESIAN_POINT('Ctrl Pts',(-87.8009595161336,-4.92340105512627,
-0.162646185699621));
#40897=CARTESIAN_POINT('Ctrl Pts',(-87.7970185112487,-4.91937734387943,
-0.243827242497861));
#40898=CARTESIAN_POINT('Ctrl Pts',(-87.7575078114986,-4.87903746823992,
-1.05771112596459));
#40899=CARTESIAN_POINT('Ctrl Pts',(-87.7179971117486,-4.63239276340937,
-1.86136959166297));
#40900=CARTESIAN_POINT('Ctrl Pts',(-87.6784864119986,-4.20922501477751,
-2.55776268860029));
#40901=CARTESIAN_POINT('Ctrl Pts',(-87.6389757122486,-3.78605726614565,
-3.25415578553761));
#40902=CARTESIAN_POINT('Ctrl Pts',(-87.5994650124986,-3.18636647371249,
-3.84328351371386));
#40903=CARTESIAN_POINT('Ctrl Pts',(-87.5599543127485,-2.48256394173379,
-4.25401004368527));
#40904=CARTESIAN_POINT('Ctrl Pts',(-87.5204436129985,-1.77876140975508,
-4.66473657365668));
#40905=CARTESIAN_POINT('Ctrl Pts',(-87.4809329132484,-0.970847138230837,
-4.89706190542324));
#40906=CARTESIAN_POINT('Ctrl Pts',(-87.4414222134984,-0.156374941776677,
-4.92293327867082));
#40907=CARTESIAN_POINT('Ctrl Pts',(-87.4019115137484,0.658097254677483,
-4.9488046519184));
#40908=CARTESIAN_POINT('Ctrl Pts',(-87.3624008139984,1.47912737606156,-4.768222066647));
#40909=CARTESIAN_POINT('Ctrl Pts',(-87.3228901142484,2.20757789747824,-4.4029904621196));
#40910=CARTESIAN_POINT('Ctrl Pts',(-87.2833794144984,2.93602841889492,-4.03775885759221));
#40911=CARTESIAN_POINT('Ctrl Pts',(-87.2438687147483,3.57189934034421,-3.48787823380882));
#40912=CARTESIAN_POINT('Ctrl Pts',(-87.2043580149983,4.03841069083489,-2.81974542771263));
#40913=CARTESIAN_POINT('Ctrl Pts',(-87.1648473152482,4.50492204132558,-2.15161262161645));
#40914=CARTESIAN_POINT('Ctrl Pts',(-87.1253366154982,4.80207382085767,-1.36522763320748));
#40915=CARTESIAN_POINT('Ctrl Pts',(-87.0858259157482,4.89398562609676,-0.555544666224829));
#40916=CARTESIAN_POINT('Ctrl Pts',(-87.0463152159981,4.98589743133585,0.254138300757821));
#40917=CARTESIAN_POINT('Ctrl Pts',(-87.0068045162482,4.87256926228193,1.08711924631414));
#40918=CARTESIAN_POINT('Ctrl Pts',(-86.9672938164981,4.56768523829136,1.84281761124461));
#40919=CARTESIAN_POINT('Ctrl Pts',(-86.9277831167481,4.26280121430078,2.59851597617508));
#40920=CARTESIAN_POINT('Ctrl Pts',(-86.888272416998,3.76636133537354,3.2769317604797));
#40921=CARTESIAN_POINT('Ctrl Pts',(-86.848761717248,3.13830959060805,3.79614779719784));
#40922=CARTESIAN_POINT('Ctrl Pts',(-86.8092510174979,2.51025784584256,4.31536383391598));
#40923=CARTESIAN_POINT('Ctrl Pts',(-86.769740317748,1.75059423523883,4.67538012304765));
#40924=CARTESIAN_POINT('Ctrl Pts',(-86.7302296179979,0.951046416362449,
4.83272551449205));
#40925=CARTESIAN_POINT('Ctrl Pts',(-86.6907189182479,0.15149859748607,4.99007090593645));
#40926=CARTESIAN_POINT('Ctrl Pts',(-86.6512082184979,-0.687933429662953,
4.94474539969359));
#40927=CARTESIAN_POINT('Ctrl Pts',(-86.6116975187478,-1.4658901522069,4.70222194778708));
#40928=CARTESIAN_POINT('Ctrl Pts',(-86.5721868189978,-2.24384687475085,
4.45969849588057));
#40929=CARTESIAN_POINT('Ctrl Pts',(-86.5326761192478,-2.96032829268972,
4.01997709831041));
#40930=CARTESIAN_POINT('Ctrl Pts',(-86.4931654194977,-3.52882090026483,
3.4361531162634));
#40931=CARTESIAN_POINT('Ctrl Pts',(-86.4536547197477,-4.09731350783993,
2.85232913421639));
#40932=CARTESIAN_POINT('Ctrl Pts',(-86.4141440199977,-4.51781730505126,
2.12440256769253));
#40933=CARTESIAN_POINT('Ctrl Pts',(-86.3746333202476,-4.73955741237156,
1.34026889816745));
#40934=CARTESIAN_POINT('Ctrl Pts',(-86.3527027221329,-4.86263529280175,
0.905031848878518));
#40935=CARTESIAN_POINT('Ctrl Pts',(-86.3307721240183,-4.92447692699912,
0.452478196132976));
#40936=CARTESIAN_POINT('Ctrl Pts',(-86.3088415259036,-4.92460788888033,
-4.03740411281871E-5));
#40937=CARTESIAN_POINT('Origin',(-74.75,0.,0.));
#40938=CARTESIAN_POINT('',(-84.5911584740964,-4.92505771915203,0.000122489528405073));
#40939=CARTESIAN_POINT('',(-84.8088415259036,-4.9250542018855,0.000122701850775453));
#40940=CARTESIAN_POINT('',(-74.75,-4.925,-6.03138548580071E-16));
#40941=CARTESIAN_POINT('Ctrl Pts',(-84.5911584740964,-4.92505771915203,
0.000122489528405073));
#40942=CARTESIAN_POINT('Ctrl Pts',(-84.5993953959038,-4.92523071445293,
0.170039545814198));
#40943=CARTESIAN_POINT('Ctrl Pts',(-84.6076323177112,-4.91660717945727,
0.339939127731318));
#40944=CARTESIAN_POINT('Ctrl Pts',(-84.6158692395186,-4.89905445633691,
0.508911150373288));
#40945=CARTESIAN_POINT('Ctrl Pts',(-84.6553799392686,-4.81485790946881,
1.31943272735152));
#40946=CARTESIAN_POINT('Ctrl Pts',(-84.6948906390186,-4.52520881587572,
2.10861200392612));
#40947=CARTESIAN_POINT('Ctrl Pts',(-84.7344013387686,-4.06508164649063,
2.78115737283848));
#40948=CARTESIAN_POINT('Ctrl Pts',(-84.7739120385187,-3.60495447710555,
3.45370274175085));
#40949=CARTESIAN_POINT('Ctrl Pts',(-84.8134227382687,-2.97434923192847,
4.00961420300098));
#40950=CARTESIAN_POINT('Ctrl Pts',(-84.8529334380187,-2.24941006367898,
4.38176670882289));
#40951=CARTESIAN_POINT('Ctrl Pts',(-84.8924441377688,-1.52447089542949,
4.7539192146448));
#40952=CARTESIAN_POINT('Ctrl Pts',(-84.9319548375188,-0.705197804107595,
4.9423127650385));
#40953=CARTESIAN_POINT('Ctrl Pts',(-84.9714655372688,0.109483843170341,
4.92419926619684));
#40954=CARTESIAN_POINT('Ctrl Pts',(-85.0109762370189,0.924165490448288,
4.90608576735518));
#40955=CARTESIAN_POINT('Ctrl Pts',(-85.0504869367689,1.73425569368228,4.68146521927817));
#40956=CARTESIAN_POINT('Ctrl Pts',(-85.0899976365189,2.44193789865959,4.27746004355608));
#40957=CARTESIAN_POINT('Ctrl Pts',(-85.129508336269,3.14962010363691,3.87345486783399));
#40958=CARTESIAN_POINT('Ctrl Pts',(-85.1690190360189,3.75489431035756,3.29006506446682));
#40959=CARTESIAN_POINT('Ctrl Pts',(-85.208529735769,4.1846750315278,2.59773362869188));
#40960=CARTESIAN_POINT('Ctrl Pts',(-85.248040435519,4.61445575269803,1.90540219291694));
#40961=CARTESIAN_POINT('Ctrl Pts',(-85.2875511352691,4.86874298831785,1.10412912473424));
#40962=CARTESIAN_POINT('Ctrl Pts',(-85.3270618350191,4.91683213158013,0.290666329302215));
#40963=CARTESIAN_POINT('Ctrl Pts',(-85.3665725347691,4.96492127484241,-0.522796466129817));
#40964=CARTESIAN_POINT('Ctrl Pts',(-85.4060832345191,4.80681232574716,-1.34844898881116));
#40965=CARTESIAN_POINT('Ctrl Pts',(-85.4455939342692,4.46159658120049,-2.08659556976164));
#40966=CARTESIAN_POINT('Ctrl Pts',(-85.4851046340192,4.11638083665383,-2.82474215071212));
#40967=CARTESIAN_POINT('Ctrl Pts',(-85.5246153337692,3.58405829665576,-3.47538278993172));
#40968=CARTESIAN_POINT('Ctrl Pts',(-85.5641260335192,2.92890570024658,-3.95995410632395));
#40969=CARTESIAN_POINT('Ctrl Pts',(-85.6036367332693,2.27375310383739,-4.44452542271619));
#40970=CARTESIAN_POINT('Ctrl Pts',(-85.6431474330193,1.49577045101708,-4.76302741628104));
#40971=CARTESIAN_POINT('Ctrl Pts',(-85.6826581327693,0.688897382127365,
-4.87700169387165));
#40972=CARTESIAN_POINT('Ctrl Pts',(-85.7221688325194,-0.117975686762337,
-4.99097597146226));
#40973=CARTESIAN_POINT('Ctrl Pts',(-85.7616795322694,-0.953739171721445,
-4.90042253307862));
#40974=CARTESIAN_POINT('Ctrl Pts',(-85.8011902320194,-1.71747652801316,
-4.61627550096966));
#40975=CARTESIAN_POINT('Ctrl Pts',(-85.8407009317694,-2.48121388430487,
-4.3321284688607));
#40976=CARTESIAN_POINT('Ctrl Pts',(-85.8802116315195,-3.17292511192919,
-3.85438784302641));
#40977=CARTESIAN_POINT('Ctrl Pts',(-85.9197223312695,-3.70908764941538,
-3.24073972020018));
#40978=CARTESIAN_POINT('Ctrl Pts',(-85.9592330310196,-4.24525018690158,
-2.62709159737394));
#40979=CARTESIAN_POINT('Ctrl Pts',(-85.9987437307696,-4.62586403424964,
-1.87753597755575));
#40980=CARTESIAN_POINT('Ctrl Pts',(-86.0382544305196,-4.80497093287972,
-1.08258000134392));
#40981=CARTESIAN_POINT('Ctrl Pts',(-86.0558891117119,-4.88491112823595,
-0.727769904557915));
#40982=CARTESIAN_POINT('Ctrl Pts',(-86.0735237929042,-4.92470961908193,
-0.363915714242581));
#40983=CARTESIAN_POINT('Ctrl Pts',(-86.0911584740964,-4.92460688967043,
-3.93952561872357E-5));
#40984=CARTESIAN_POINT('Ctrl Pts',(-86.3088415259036,-4.92460788888033,
-4.03740411281871E-5));
#40985=CARTESIAN_POINT('Ctrl Pts',(-86.2912614242683,-4.92471287111428,
-0.362790282362978));
#40986=CARTESIAN_POINT('Ctrl Pts',(-86.273681322633,-4.88516247587605,-0.725517646567889));
#40987=CARTESIAN_POINT('Ctrl Pts',(-86.2561012209976,-4.80571231438,-1.07928417758196));
#40988=CARTESIAN_POINT('Ctrl Pts',(-86.2165905212476,-4.62715069163887,
-1.87436281128003));
#40989=CARTESIAN_POINT('Ctrl Pts',(-86.1770798214975,-4.24705102872735,
-2.62417930614987));
#40990=CARTESIAN_POINT('Ctrl Pts',(-86.1375691217475,-3.71130949762144,
-3.2381950215242));
#40991=CARTESIAN_POINT('Ctrl Pts',(-86.0980584219974,-3.17556796651552,
-3.85221073689853));
#40992=CARTESIAN_POINT('Ctrl Pts',(-86.0585477222474,-2.4841845672152,-4.33042567277734));
#40993=CARTESIAN_POINT('Ctrl Pts',(-86.0190370224974,-1.72064227666466,
-4.6150964605646));
#40994=CARTESIAN_POINT('Ctrl Pts',(-85.9795263227474,-0.957099986114123,
-4.89976724835186));
#40995=CARTESIAN_POINT('Ctrl Pts',(-85.9400156229973,-0.121398804313364,
-4.99089388804757));
#40996=CARTESIAN_POINT('Ctrl Pts',(-85.9005049232473,0.685552246965759,
-4.87747304464519));
#40997=CARTESIAN_POINT('Ctrl Pts',(-85.8609942234973,1.49250329824487,-4.76405220124282));
#40998=CARTESIAN_POINT('Ctrl Pts',(-85.8214835237472,2.27070421900234,-4.44608387474238));
#40999=CARTESIAN_POINT('Ctrl Pts',(-85.7819728239972,2.92618901353828,-3.9619620192032));
#41000=CARTESIAN_POINT('Ctrl Pts',(-85.7424621242472,3.58167380807422,-3.47784016366402));
#41001=CARTESIAN_POINT('Ctrl Pts',(-85.7029514244972,4.11444247638863,-2.82756477908611));
#41002=CARTESIAN_POINT('Ctrl Pts',(-85.6634407247471,4.4601644104591,-2.08965514289672));
#41003=CARTESIAN_POINT('Ctrl Pts',(-85.6239300249971,4.80588634452957,-1.35174550670734));
#41004=CARTESIAN_POINT('Ctrl Pts',(-85.5844193252471,4.9645615443561,-0.526201618906478));
#41005=CARTESIAN_POINT('Ctrl Pts',(-85.544908625497,4.91703033954142,0.287293968941061));
#41006=CARTESIAN_POINT('Ctrl Pts',(-85.505397925747,4.86949913472673,1.1007895567886));
#41007=CARTESIAN_POINT('Ctrl Pts',(-85.465887225997,4.61576152527082,1.90223684468283));
#41008=CARTESIAN_POINT('Ctrl Pts',(-85.426376526247,4.18645575186844,2.59486289083034));
#41009=CARTESIAN_POINT('Ctrl Pts',(-85.386865826497,3.75714997846606,3.28748893697786));
#41010=CARTESIAN_POINT('Ctrl Pts',(-85.3473551267469,3.15227604111722,3.87129374137866));
#41011=CARTESIAN_POINT('Ctrl Pts',(-85.3078444269969,2.44487109549709,4.27578419836216));
#41012=CARTESIAN_POINT('Ctrl Pts',(-85.2683337272468,1.73746614987695,4.68027465534567));
#41013=CARTESIAN_POINT('Ctrl Pts',(-85.2288230274968,0.927530195985523,
4.90545076491186));
#41014=CARTESIAN_POINT('Ctrl Pts',(-85.1893123277468,0.112861162777333,
4.92412302268102));
#41015=CARTESIAN_POINT('Ctrl Pts',(-85.1498016279967,-0.701807870430851,
4.94279528045018));
#41016=CARTESIAN_POINT('Ctrl Pts',(-85.1102909282467,-1.5212099829558,4.75496368642231));
#41017=CARTESIAN_POINT('Ctrl Pts',(-85.0707802284967,-2.24640422866356,
4.38330847944828));
#41018=CARTESIAN_POINT('Ctrl Pts',(-85.0312695287467,-2.97159847437131,
4.01165327247425));
#41019=CARTESIAN_POINT('Ctrl Pts',(-84.9917588289967,-3.60258485326187,
3.45617445255406));
#41020=CARTESIAN_POINT('Ctrl Pts',(-84.9522481292466,-4.06317319158446,
2.78394482699462));
#41021=CARTESIAN_POINT('Ctrl Pts',(-84.9127374294966,-4.52376152990704,
2.11171520143517));
#41022=CARTESIAN_POINT('Ctrl Pts',(-84.8732267297466,-4.81395182766163,
1.32273477023646));
#41023=CARTESIAN_POINT('Ctrl Pts',(-84.8337160299966,-4.89870426474054,
0.51227113052908));
#41024=CARTESIAN_POINT('Ctrl Pts',(-84.8254245286322,-4.91648995196233,
0.342191622525732));
#41025=CARTESIAN_POINT('Ctrl Pts',(-84.8171330272679,-4.92522837245193,
0.171166016675559));
#41026=CARTESIAN_POINT('Ctrl Pts',(-84.8088415259036,-4.9250542018855,0.000122701850775453));
#41027=CARTESIAN_POINT('Origin',(-74.75,0.,0.));
#41028=CARTESIAN_POINT('',(-83.0911584740965,-4.92523349004336,-9.88184705141837E-5));
#41029=CARTESIAN_POINT('',(-83.3088415259037,-4.92523661103536,-9.81287755307904E-5));
#41030=CARTESIAN_POINT('',(-74.75,-4.925,-6.03138548580071E-16));
#41031=CARTESIAN_POINT('Ctrl Pts',(-83.0911584740965,-4.92523349004336,
-9.88184705141837E-5));
#41032=CARTESIAN_POINT('Ctrl Pts',(-83.1252669989035,-4.92459715090507,
0.70344350101895));
#41033=CARTESIAN_POINT('Ctrl Pts',(-83.1593755237105,-4.77223537727082,
1.40725258976148));
#41034=CARTESIAN_POINT('Ctrl Pts',(-83.1934840485175,-4.47986315706691,
2.04708358868986));
#41035=CARTESIAN_POINT('Ctrl Pts',(-83.2329947482675,-4.14118445216601,
2.78825227400949));
#41036=CARTESIAN_POINT('Ctrl Pts',(-83.2725054480176,-3.61463290306591,
3.44357203880708));
#41037=CARTESIAN_POINT('Ctrl Pts',(-83.3120161477676,-2.96378841474844,
3.93391450818797));
#41038=CARTESIAN_POINT('Ctrl Pts',(-83.3515268475176,-2.31294392643097,
4.42425697756886));
#41039=CARTESIAN_POINT('Ctrl Pts',(-83.3910375472677,-1.53780649889613,
4.74962215153305));
#41040=CARTESIAN_POINT('Ctrl Pts',(-83.4305482470177,-0.731972217987289,
4.87072292347077));
#41041=CARTESIAN_POINT('Ctrl Pts',(-83.4700589467677,0.0738620629215621,
4.99182369540848));
#41042=CARTESIAN_POINT('Ctrl Pts',(-83.5095696465177,0.910393197204418,
4.90866006531972));
#41043=CARTESIAN_POINT('Ctrl Pts',(-83.5490803462678,1.67661194821018,4.6312738528668));
#41044=CARTESIAN_POINT('Ctrl Pts',(-83.5885910460178,2.44283069921593,4.35388764041389));
#41045=CARTESIAN_POINT('Ctrl Pts',(-83.6281017457678,3.1387370669446,3.88227884559683));
#41046=CARTESIAN_POINT('Ctrl Pts',(-83.6676124455178,3.68030193627522,3.2733931604648));
#41047=CARTESIAN_POINT('Ctrl Pts',(-83.7071231452679,4.22186680560584,2.66450747533277));
#41048=CARTESIAN_POINT('Ctrl Pts',(-83.7466338450179,4.60909017653842,1.91834489988576));
#41049=CARTESIAN_POINT('Ctrl Pts',(-83.786144544768,4.79521570551511,1.12500287231193));
#41050=CARTESIAN_POINT('Ctrl Pts',(-83.825655244518,4.9813412344918,0.33166084473811));
#41051=CARTESIAN_POINT('Ctrl Pts',(-83.865165944268,4.96636892151259,-0.508860634962529));
#41052=CARTESIAN_POINT('Ctrl Pts',(-83.9046766440181,4.7521066394025,-1.29507050498247));
#41053=CARTESIAN_POINT('Ctrl Pts',(-83.9441873437681,4.5378443572924,-2.0812803750024));
#41054=CARTESIAN_POINT('Ctrl Pts',(-83.9836980435181,4.12429210605142,-2.81317863534163));
#41055=CARTESIAN_POINT('Ctrl Pts',(-84.0232087432682,3.56138538180307,-3.40239023150024));
#41056=CARTESIAN_POINT('Ctrl Pts',(-84.0627194430182,2.99847865755472,-3.99160182765885));
#41057=CARTESIAN_POINT('Ctrl Pts',(-84.1022301427682,2.286217460299,-4.43812675963685));
#41058=CARTESIAN_POINT('Ctrl Pts',(-84.1417408425183,1.51060571371853,-4.68804815491584));
#41059=CARTESIAN_POINT('Ctrl Pts',(-84.1812515422683,0.734993967138068,
-4.93796955019483));
#41060=CARTESIAN_POINT('Ctrl Pts',(-84.2207622420183,-0.103968328767144,
-4.99128740877481));
#41061=CARTESIAN_POINT('Ctrl Pts',(-84.2602729417683,-0.90497838009561,
-4.84156372019293));
#41062=CARTESIAN_POINT('Ctrl Pts',(-84.2997836415183,-1.70598843142406,
-4.69184003161104));
#41063=CARTESIAN_POINT('Ctrl Pts',(-84.3392943412683,-2.46904623817577,
-4.33907479586728));
#41064=CARTESIAN_POINT('Ctrl Pts',(-84.3788050410184,-3.10201430131225,
-3.82586361486961));
#41065=CARTESIAN_POINT('Ctrl Pts',(-84.4183157407684,-3.73498236444874,
-3.31265243387192));
#41066=CARTESIAN_POINT('Ctrl Pts',(-84.4578264405184,-4.23786068397,-2.6389953076203));
#41067=CARTESIAN_POINT('Ctrl Pts',(-84.4973371402685,-4.54992784365907,
-1.88623480580356));
#41068=CARTESIAN_POINT('Ctrl Pts',(-84.5286109182111,-4.79693736556213,
-1.2904046907523));
#41069=CARTESIAN_POINT('Ctrl Pts',(-84.5598846961538,-4.92440089409629,
-0.645015149412324));
#41070=CARTESIAN_POINT('Ctrl Pts',(-84.5911584740964,-4.92505771915203,
0.000122489528405073));
#41071=CARTESIAN_POINT('Ctrl Pts',(-84.8088415259036,-4.9250542018855,0.000122701850775453));
#41072=CARTESIAN_POINT('Ctrl Pts',(-84.7776223275179,-4.92439841408211,
-0.643890359650401));
#41073=CARTESIAN_POINT('Ctrl Pts',(-84.7464031291322,-4.79739091687878,
-1.28815447712395));
#41074=CARTESIAN_POINT('Ctrl Pts',(-84.7151839307465,-4.55122048505408,
-1.88311371961037));
#41075=CARTESIAN_POINT('Ctrl Pts',(-84.6756732309964,-4.23966969188548,
-2.63608808182635));
#41076=CARTESIAN_POINT('Ctrl Pts',(-84.6361625312464,-3.73725352914504,
-3.31008995804226));
#41077=CARTESIAN_POINT('Ctrl Pts',(-84.5966518314964,-3.10463760866692,
-3.82373515079322));
#41078=CARTESIAN_POINT('Ctrl Pts',(-84.5571411317463,-2.4720216881888,-4.33738034354418));
#41079=CARTESIAN_POINT('Ctrl Pts',(-84.5176304319963,-1.70920600997301,
-4.6906688528302));
#41080=CARTESIAN_POINT('Ctrl Pts',(-84.4781197322463,-0.908298836586612,
-4.84094189265024));
#41081=CARTESIAN_POINT('Ctrl Pts',(-84.4386090324963,-0.107391663200203,
-4.99121493247029));
#41082=CARTESIAN_POINT('Ctrl Pts',(-84.3990983327462,0.731607005356798,
-4.93847250282434));
#41083=CARTESIAN_POINT('Ctrl Pts',(-84.3595876329962,1.50738998326773,-4.68908313243696));
#41084=CARTESIAN_POINT('Ctrl Pts',(-84.3200769332462,2.28317296117865,-4.43969376204958));
#41085=CARTESIAN_POINT('Ctrl Pts',(-84.2805662334961,2.99574024844349,-3.99365745092077));
#41086=CARTESIAN_POINT('Ctrl Pts',(-84.2410555337461,3.55905096170545,-3.40483207170988));
#41087=CARTESIAN_POINT('Ctrl Pts',(-84.2015448339961,4.12236167496742,-2.81600669249899));
#41088=CARTESIAN_POINT('Ctrl Pts',(-84.162034134246,4.53641581422651,-2.084392245206));
#41089=CARTESIAN_POINT('Ctrl Pts',(-84.122523434496,4.75121728151961,-1.29832951454941));
#41090=CARTESIAN_POINT('Ctrl Pts',(-84.0830127347459,4.96601874881271,-0.512266783892823));
#41091=CARTESIAN_POINT('Ctrl Pts',(-84.043502034996,4.98156754413983,0.32824423012738));
#41092=CARTESIAN_POINT('Ctrl Pts',(-84.0039913352459,4.79598618574032,1.12171372941084));
#41093=CARTESIAN_POINT('Ctrl Pts',(-83.964480635496,4.6104048273408,1.9151832286943));
#41094=CARTESIAN_POINT('Ctrl Pts',(-83.9249699357459,4.22369331521466,2.66161121324101));
#41095=CARTESIAN_POINT('Ctrl Pts',(-83.8854592359959,3.68254618713009,3.27086819731618));
#41096=CARTESIAN_POINT('Ctrl Pts',(-83.8459485362458,3.14139905904551,3.88012518139135));
#41097=CARTESIAN_POINT('Ctrl Pts',(-83.8064378364957,2.44581631500251,4.35221116499496));
#41098=CARTESIAN_POINT('Ctrl Pts',(-83.7669271367457,1.67978799329618,4.63012283661445));
#41099=CARTESIAN_POINT('Ctrl Pts',(-83.7274164369957,0.91375967158985,4.90803450823395));
#41100=CARTESIAN_POINT('Ctrl Pts',(-83.6879057372457,0.0772857722201863,
4.99177186786932));
#41101=CARTESIAN_POINT('Ctrl Pts',(-83.6483950374957,-0.728631379147621,
4.87122381931709));
#41102=CARTESIAN_POINT('Ctrl Pts',(-83.6088843377457,-1.53454853051542,
4.75067577076485));
#41103=CARTESIAN_POINT('Ctrl Pts',(-83.5693736379956,-2.30990893388137,
4.42584231402501));
#41104=CARTESIAN_POINT('Ctrl Pts',(-83.5298629382456,-2.96108957957636,
3.9359463520588));
#41105=CARTESIAN_POINT('Ctrl Pts',(-83.4903522384955,-3.61227022527137,
3.44605039009258));
#41106=CARTESIAN_POINT('Ctrl Pts',(-83.4508415387455,-4.13927111329541,
2.79109192289997));
#41107=CARTESIAN_POINT('Ctrl Pts',(-83.4113308389955,-4.47845808201097,
2.05015569950951));
#41108=CARTESIAN_POINT('Ctrl Pts',(-83.3771677346316,-4.77173762108358,
1.40950185923659));
#41109=CARTESIAN_POINT('Ctrl Pts',(-83.3430046302676,-4.92460232693747,
0.704568692162481));
#41110=CARTESIAN_POINT('Ctrl Pts',(-83.3088415259037,-4.92523661103536,
-9.81287755307904E-5));
#41111=CARTESIAN_POINT('Origin',(-74.75,0.,0.));
#41112=CARTESIAN_POINT('',(-81.5911584740964,-4.92458990475544,-1.34620480526926E-5));
#41113=CARTESIAN_POINT('',(-81.8088415259037,-4.92459025730219,-1.44866882854098E-5));
#41114=CARTESIAN_POINT('',(-74.75,-4.925,-6.03138548580071E-16));
#41115=CARTESIAN_POINT('Ctrl Pts',(-81.5911584740964,-4.92458990475544,
-1.34620480526926E-5));
#41116=CARTESIAN_POINT('Ctrl Pts',(-81.6116279021531,-4.92454933037037,
0.422359563629195));
#41117=CARTESIAN_POINT('Ctrl Pts',(-81.6320973302098,-4.87076599946272,
0.844742733033155));
#41118=CARTESIAN_POINT('Ctrl Pts',(-81.6525667582664,-4.7633665661891,1.25302197955212));
#41119=CARTESIAN_POINT('Ctrl Pts',(-81.6920774580165,-4.55606098101821,
2.04109474244191));
#41120=CARTESIAN_POINT('Ctrl Pts',(-81.7315881577664,-4.14899321709825,
2.77661929238658));
#41121=CARTESIAN_POINT('Ctrl Pts',(-81.7710988575164,-3.5913157834199,3.37078270864319));
#41122=CARTESIAN_POINT('Ctrl Pts',(-81.8106095572665,-3.03363834974155,
3.9649461248998));
#41123=CARTESIAN_POINT('Ctrl Pts',(-81.8501202570166,-2.32535124630482,
4.41774840746836));
#41124=CARTESIAN_POINT('Ctrl Pts',(-81.8896309567666,-1.55197853397958,
4.67451470798793));
#41125=CARTESIAN_POINT('Ctrl Pts',(-81.9291416565166,-0.77860582165434,
4.93128100850749));
#41126=CARTESIAN_POINT('Ctrl Pts',(-81.9686523562666,0.059852499559401,
4.99201132697805));
#41127=CARTESIAN_POINT('Ctrl Pts',(-82.0081630560166,0.862154489560794,
4.84937261522138));
#41128=CARTESIAN_POINT('Ctrl Pts',(-82.0476737557666,1.66445647956217,4.70673390346471));
#41129=CARTESIAN_POINT('Ctrl Pts',(-82.0871844555167,2.43060213835121,4.36072616148081));
#41130=CARTESIAN_POINT('Ctrl Pts',(-82.1266951552668,3.06808111576122,3.85312903913666));
#41131=CARTESIAN_POINT('Ctrl Pts',(-82.1662058550168,3.70556009317124,3.34553191679251));
#41132=CARTESIAN_POINT('Ctrl Pts',(-82.2057165547668,4.21437238920223,2.67634541408811));
#41133=CARTESIAN_POINT('Ctrl Pts',(-82.2452272545168,4.53308007343595,1.9263722830613));
#41134=CARTESIAN_POINT('Ctrl Pts',(-82.2847379542668,4.85178775766967,1.17639915203446));
#41135=CARTESIAN_POINT('Ctrl Pts',(-82.3242486540168,4.98039083010609,0.345639392685209));
#41136=CARTESIAN_POINT('Ctrl Pts',(-82.3637593537669,4.90336076150653,-0.46559463876525));
#41137=CARTESIAN_POINT('Ctrl Pts',(-82.4032700535169,4.82633069290697,-1.27682867021569));
#41138=CARTESIAN_POINT('Ctrl Pts',(-82.442780753267,4.54366748327143,-2.06853697376733));
#41139=CARTESIAN_POINT('Ctrl Pts',(-82.482291453017,4.0895020738937,-2.74512256789163));
#41140=CARTESIAN_POINT('Ctrl Pts',(-82.521802152767,3.63533666451597,-3.42170816201595));
#41141=CARTESIAN_POINT('Ctrl Pts',(-82.5613128525171,3.00966905539604,-3.98317104671292));
#41142=CARTESIAN_POINT('Ctrl Pts',(-82.6008235522671,2.28804719090147,-4.36171585242972));
#41143=CARTESIAN_POINT('Ctrl Pts',(-82.6403342520171,1.56642532640689,-4.74026065814652));
#41144=CARTESIAN_POINT('Ctrl Pts',(-82.6798449517671,0.748849206537666,
-4.93588738488314));
#41145=CARTESIAN_POINT('Ctrl Pts',(-82.7193556515172,-0.0659607070428713,
-4.92497454919873));
#41146=CARTESIAN_POINT('Ctrl Pts',(-82.7588663512672,-0.88077062062342,
-4.91406171351432));
#41147=CARTESIAN_POINT('Ctrl Pts',(-82.7983770510173,-1.69281432791528,
-4.69660931540887));
#41148=CARTESIAN_POINT('Ctrl Pts',(-82.8378877507673,-2.40403939352261,
-4.29887423862577));
#41149=CARTESIAN_POINT('Ctrl Pts',(-82.8773984505173,-3.11526445912993,
-3.90113916184267));
#41150=CARTESIAN_POINT('Ctrl Pts',(-82.9169091502673,-3.72567088305271,
-3.32312140638193));
#41151=CARTESIAN_POINT('Ctrl Pts',(-82.9564198500173,-4.16155347441339,
-2.63461530488356));
#41152=CARTESIAN_POINT('Ctrl Pts',(-82.9959305497674,-4.59743606577406,
-1.94610920338519));
#41153=CARTESIAN_POINT('Ctrl Pts',(-83.0354412495174,-4.85879482457262,
-1.14711475584919));
#41154=CARTESIAN_POINT('Ctrl Pts',(-83.0749519492675,-4.91407127362106,
-0.334108729160355));
#41155=CARTESIAN_POINT('Ctrl Pts',(-83.0803541242105,-4.92162905037208,
-0.222948946780624));
#41156=CARTESIAN_POINT('Ctrl Pts',(-83.0857562991535,-4.92533427468202,
-0.1115272285582));
#41157=CARTESIAN_POINT('Ctrl Pts',(-83.0911584740965,-4.92523349004336,
-9.88184705141837E-5));
#41158=CARTESIAN_POINT('Ctrl Pts',(-83.3088415259037,-4.92523661103536,
-9.81287755307904E-5));
#41159=CARTESIAN_POINT('Ctrl Pts',(-83.3034939305176,-4.92533589635437,
-0.110400547438018));
#41160=CARTESIAN_POINT('Ctrl Pts',(-83.2981463351315,-4.9217052242449,-0.220696440074123));
#41161=CARTESIAN_POINT('Ctrl Pts',(-83.2927987397455,-4.91429927793192,
-0.330738252215514));
#41162=CARTESIAN_POINT('Ctrl Pts',(-83.2532880399954,-4.85958045573022,
-1.14378200096181));
#41163=CARTESIAN_POINT('Ctrl Pts',(-83.2137773402453,-4.59876976191972,
-1.94295551886606));
#41164=CARTESIAN_POINT('Ctrl Pts',(-83.1742666404953,-4.1633594960845,-2.63176041670279));
#41165=CARTESIAN_POINT('Ctrl Pts',(-83.1347559407453,-3.72794923024929,
-3.32056531453952));
#41166=CARTESIAN_POINT('Ctrl Pts',(-83.0952452409953,-3.11793939238936,
-3.89900159230872));
#41167=CARTESIAN_POINT('Ctrl Pts',(-83.0557345412453,-2.40698728651493,
-4.29722438175111));
#41168=CARTESIAN_POINT('Ctrl Pts',(-83.0162238414952,-1.69603518064051,
-4.69544717119349));
#41169=CARTESIAN_POINT('Ctrl Pts',(-82.9767131417452,-0.884140806751607,
-4.91345647230907));
#41170=CARTESIAN_POINT('Ctrl Pts',(-82.9372024419952,-0.0693385685744247,
-4.92492815657942));
#41171=CARTESIAN_POINT('Ctrl Pts',(-82.8976917422451,0.74546366960277,-4.93639984084977));
#41172=CARTESIAN_POINT('Ctrl Pts',(-82.858181042495,1.56317377206823,-4.74133390827489));
#41173=CARTESIAN_POINT('Ctrl Pts',(-82.818670342745,2.2850550990641,-4.36328412767286));
#41174=CARTESIAN_POINT('Ctrl Pts',(-82.779159642995,3.00693642605996,-3.98523434707082));
#41175=CARTESIAN_POINT('Ctrl Pts',(-82.739648943245,3.63298897758623,-3.42420071844163));
#41176=CARTESIAN_POINT('Ctrl Pts',(-82.700138243495,4.0876183283531,-2.74792677964179));
#41177=CARTESIAN_POINT('Ctrl Pts',(-82.660627543745,4.54224767911996,-2.07165284084196));
#41178=CARTESIAN_POINT('Ctrl Pts',(-82.6211168439949,4.82545382912743,-1.28013859187147));
#41179=CARTESIAN_POINT('Ctrl Pts',(-82.5816061442449,4.90304027826355,-0.468957582608441));
#41180=CARTESIAN_POINT('Ctrl Pts',(-82.5420954444948,4.98062672739968,0.342223426654603));
#41181=CARTESIAN_POINT('Ctrl Pts',(-82.5025847447448,4.85259347566446,1.17307119621018));
#41182=CARTESIAN_POINT('Ctrl Pts',(-82.4630740449948,4.53440024773965,1.92326274280435));
#41183=CARTESIAN_POINT('Ctrl Pts',(-82.4235633452448,4.21620701981484,2.67345428939852));
#41184=CARTESIAN_POINT('Ctrl Pts',(-82.3840526454948,3.70785381570044,3.34298961303128));
#41185=CARTESIAN_POINT('Ctrl Pts',(-82.3445419457448,3.07072313150732,3.85102384232903));
#41186=CARTESIAN_POINT('Ctrl Pts',(-82.3050312459947,2.43359244731419,4.35905807162678));
#41187=CARTESIAN_POINT('Ctrl Pts',(-82.2655205462446,1.66768428304235,4.70559120658953));
#41188=CARTESIAN_POINT('Ctrl Pts',(-82.2260098464946,0.865480311934301,
4.84878015734007));
#41189=CARTESIAN_POINT('Ctrl Pts',(-82.1864991467446,0.0632763408262584,
4.9919691080906));
#41190=CARTESIAN_POINT('Ctrl Pts',(-82.1469884469946,-0.775223437117998,
4.93181387462891));
#41191=CARTESIAN_POINT('Ctrl Pts',(-82.1074777472446,-1.54877207599144,
4.67557806492309));
#41192=CARTESIAN_POINT('Ctrl Pts',(-82.0679670474946,-2.32232071486487,
4.41934225521726));
#41193=CARTESIAN_POINT('Ctrl Pts',(-82.0284563477445,-3.0309182146675,3.9670258692673));
#41194=CARTESIAN_POINT('Ctrl Pts',(-81.9889456479944,-3.58900303487245,
3.37324508451981));
#41195=CARTESIAN_POINT('Ctrl Pts',(-81.9494349482444,-4.14708785507741,
2.7794642997723));
#41196=CARTESIAN_POINT('Ctrl Pts',(-81.9099242484944,-4.55465999568467,
2.04421911622726));
#41197=CARTESIAN_POINT('Ctrl Pts',(-81.8704135487444,-4.76250604536285,
1.25628872176862));
#41198=CARTESIAN_POINT('Ctrl Pts',(-81.8498895411308,-4.87047259450106,
0.846994795891583));
#41199=CARTESIAN_POINT('Ctrl Pts',(-81.8293655335172,-4.92454647447177,
0.423484667070903));
#41200=CARTESIAN_POINT('Ctrl Pts',(-81.8088415259037,-4.92459025730219,
-1.44866882854098E-5));
#41201=CARTESIAN_POINT('Origin',(-74.75,0.,0.));
#41202=CARTESIAN_POINT('',(-80.0911584740964,-4.92514750914162,0.000113799890342631));
#41203=CARTESIAN_POINT('',(-80.3088415259036,-4.92514409493932,0.00011425152402452));
#41204=CARTESIAN_POINT('',(-74.75,-4.925,-6.03138548580071E-16));
#41205=CARTESIAN_POINT('Ctrl Pts',(-80.0911584740964,-4.92514750914162,
0.000113799890342631));
#41206=CARTESIAN_POINT('Ctrl Pts',(-80.0979888054027,-4.92528677249564,
0.141007302869867));
#41207=CARTESIAN_POINT('Ctrl Pts',(-80.104819136709,-4.91936056283244,0.281889128591955));
#41208=CARTESIAN_POINT('Ctrl Pts',(-80.1116494680152,-4.90728407783657,
0.42224176076328));
#41209=CARTESIAN_POINT('Ctrl Pts',(-80.1511601677652,-4.83742650412431,
1.23412488329213));
#41210=CARTESIAN_POINT('Ctrl Pts',(-80.1906708675153,-4.56177125654089,
2.02830037553067));
#41211=CARTESIAN_POINT('Ctrl Pts',(-80.2301815672654,-4.1136030808575,2.70887334851438));
#41212=CARTESIAN_POINT('Ctrl Pts',(-80.2696922670154,-3.6654349051741,3.3894463214981));
#41213=CARTESIAN_POINT('Ctrl Pts',(-80.3092029667654,-3.04475380139071,
3.95641677522698));
#41214=CARTESIAN_POINT('Ctrl Pts',(-80.3487136665154,-2.32650560467001,
4.34132431368209));
#41215=CARTESIAN_POINT('Ctrl Pts',(-80.3882243662655,-1.60825740794929,
4.72623185213721));
#41216=CARTESIAN_POINT('Ctrl Pts',(-80.4277350660155,-0.792442118291283,
4.92907647531854));
#41217=CARTESIAN_POINT('Ctrl Pts',(-80.4672457657655,0.0224324188948811,
4.92536515516476));
#41218=CARTESIAN_POINT('Ctrl Pts',(-80.5067564655156,0.837306956081022,
4.92165383501097));
#41219=CARTESIAN_POINT('Ctrl Pts',(-80.5462671652656,1.65124074079532,4.71138657152206));
#41220=CARTESIAN_POINT('Ctrl Pts',(-80.5857778650156,2.36595311508063,4.31995265973708));
#41221=CARTESIAN_POINT('Ctrl Pts',(-80.6252885647656,3.08066548936595,3.92851874795209));
#41222=CARTESIAN_POINT('Ctrl Pts',(-80.6647992645157,3.69615645322232,3.35591818787104));
#41223=CARTESIAN_POINT('Ctrl Pts',(-80.7043099642657,4.13810686911053,2.67129119808172));
#41224=CARTESIAN_POINT('Ctrl Pts',(-80.7438206640157,4.58005728499876,1.98666420829237));
#41225=CARTESIAN_POINT('Ctrl Pts',(-80.7833313637658,4.84846715291882,1.19001078879474));
#41226=CARTESIAN_POINT('Ctrl Pts',(-80.8228420635158,4.91092659025283,0.377525032648988));
#41227=CARTESIAN_POINT('Ctrl Pts',(-80.8623527632658,4.97338602758685,-0.434960723496752));
#41228=CARTESIAN_POINT('Ctrl Pts',(-80.9018634630158,4.82989503433481,-1.26327881629061));
#41229=CARTESIAN_POINT('Ctrl Pts',(-80.9413741627658,4.49777982239817,-2.0074117152086));
#41230=CARTESIAN_POINT('Ctrl Pts',(-80.9808848625159,4.16566461046152,-2.75154461412658));
#41231=CARTESIAN_POINT('Ctrl Pts',(-81.0203955622659,3.64492517984028,-3.41149231916869));
#41232=CARTESIAN_POINT('Ctrl Pts',(-81.059906262016,2.9984396353957,-3.90756764215502));
#41233=CARTESIAN_POINT('Ctrl Pts',(-81.099416961766,2.35195409095114,-4.40364296514134));
#41234=CARTESIAN_POINT('Ctrl Pts',(-81.138927661516,1.57972243268324,-4.7358459060719));
#41235=CARTESIAN_POINT('Ctrl Pts',(-81.178438361266,0.774989881388653,-4.86406371348835));
#41236=CARTESIAN_POINT('Ctrl Pts',(-81.2179490610161,-0.0297426699059256,
-4.99228152090479));
#41237=CARTESIAN_POINT('Ctrl Pts',(-81.2574597607661,-0.8669761142272,-4.91651419480714));
#41238=CARTESIAN_POINT('Ctrl Pts',(-81.2969704605161,-1.63561641258026,
-4.64591046793058));
#41239=CARTESIAN_POINT('Ctrl Pts',(-81.3364811602662,-2.40425671093334,
-4.37530674105401));
#41240=CARTESIAN_POINT('Ctrl Pts',(-81.3759918600162,-3.1043038633182,-3.90986661339851));
#41241=CARTESIAN_POINT('Ctrl Pts',(-81.4155025597662,-3.65122876426073,
-3.30579092444817));
#41242=CARTESIAN_POINT('Ctrl Pts',(-81.4550132595162,-4.19815366520325,
-2.70171523549784));
#41243=CARTESIAN_POINT('Ctrl Pts',(-81.4945239592662,-4.59195631470344,
-1.95900398525268));
#41244=CARTESIAN_POINT('Ctrl Pts',(-81.5340346590163,-4.78508593624262,
-1.16733787221264));
#41245=CARTESIAN_POINT('Ctrl Pts',(-81.5530759307097,-4.87816030898299,
-0.78581262350264));
#41246=CARTESIAN_POINT('Ctrl Pts',(-81.572117202403,-4.924627648257,-0.392917431597961));
#41247=CARTESIAN_POINT('Ctrl Pts',(-81.5911584740964,-4.92458990475544,
-1.34620480526926E-5));
#41248=CARTESIAN_POINT('Ctrl Pts',(-81.8088415259037,-4.92459025730219,
-1.44866882854098E-5));
#41249=CARTESIAN_POINT('Ctrl Pts',(-81.7898548337672,-4.92463076065503,
-0.391792164998725));
#41250=CARTESIAN_POINT('Ctrl Pts',(-81.7708681416308,-4.8784320938656,-0.783560450808273));
#41251=CARTESIAN_POINT('Ctrl Pts',(-81.7518814494943,-4.78588545501263,
-1.16405566707921));
#41252=CARTESIAN_POINT('Ctrl Pts',(-81.7123707497443,-4.59329885623518,
-1.95585405609618));
#41253=CARTESIAN_POINT('Ctrl Pts',(-81.6728600499942,-4.20000569993118,
-2.69883522875792));
#41254=CARTESIAN_POINT('Ctrl Pts',(-81.6333493502442,-3.65349524247176,
-3.30328589404503));
#41255=CARTESIAN_POINT('Ctrl Pts',(-81.5938386504941,-3.10698478501233,
-3.90773655933216));
#41256=CARTESIAN_POINT('Ctrl Pts',(-81.5543279507441,-2.40725702639747,
-4.37365671724465));
#41257=CARTESIAN_POINT('Ctrl Pts',(-81.5148172509941,-1.63880250602815,
-4.64478756573394));
#41258=CARTESIAN_POINT('Ctrl Pts',(-81.4753065512441,-0.87034798565884,
-4.91591841422321));
#41259=CARTESIAN_POINT('Ctrl Pts',(-81.4357958514941,-0.0331667035350426,
-4.99225995328928));
#41260=CARTESIAN_POINT('Ctrl Pts',(-81.3962851517441,0.771653599815262,
-4.86459411528371));
#41261=CARTESIAN_POINT('Ctrl Pts',(-81.356774451994,1.57647390316558,-4.73692827727813));
#41262=CARTESIAN_POINT('Ctrl Pts',(-81.3172637522439,2.34893322774243,-4.40525506220092));
#41263=CARTESIAN_POINT('Ctrl Pts',(-81.2777530524939,2.9957588625589,-3.90962325831537));
#41264=CARTESIAN_POINT('Ctrl Pts',(-81.2382423527439,3.64258449737536,-3.41399145442983));
#41265=CARTESIAN_POINT('Ctrl Pts',(-81.1987316529939,4.16377644243144,-2.75440106173597));
#41266=CARTESIAN_POINT('Ctrl Pts',(-81.1592209532439,4.49640195277443,-2.01049612375826));
#41267=CARTESIAN_POINT('Ctrl Pts',(-81.1197102534938,4.82902746311742,-1.26659118578055));
#41268=CARTESIAN_POINT('Ctrl Pts',(-81.0801995537438,4.97308653874732,-0.438371702519009));
#41269=CARTESIAN_POINT('Ctrl Pts',(-81.0406888539937,4.91118437310442,0.374156702379712));
#41270=CARTESIAN_POINT('Ctrl Pts',(-81.0011781542437,4.84928220746151,1.18668510727843));
#41271=CARTESIAN_POINT('Ctrl Pts',(-80.9616674544937,4.5814188005458,1.98352243381432));
#41272=CARTESIAN_POINT('Ctrl Pts',(-80.9221567547437,4.13993805104853,2.66845238256957));
#41273=CARTESIAN_POINT('Ctrl Pts',(-80.8826460549936,3.69845730155124,3.35338233132484));
#41274=CARTESIAN_POINT('Ctrl Pts',(-80.8431353552436,3.08335920947238,3.92640490229945));
#41275=CARTESIAN_POINT('Ctrl Pts',(-80.8036246554936,2.36891547397553,4.31832892004766));
#41276=CARTESIAN_POINT('Ctrl Pts',(-80.7641139557436,1.65447173847872,4.71025293779585));
#41277=CARTESIAN_POINT('Ctrl Pts',(-80.7246032559935,0.840682359563916,
4.92107840231764));
#41278=CARTESIAN_POINT('Ctrl Pts',(-80.6850925562435,0.0258105585151022,
4.92534861706558));
#41279=CARTESIAN_POINT('Ctrl Pts',(-80.6455818564935,-0.789061242533735,
4.92961883181351));
#41280=CARTESIAN_POINT('Ctrl Pts',(-80.6060711567434,-1.6050154657166,4.72733379678758));
#41281=CARTESIAN_POINT('Ctrl Pts',(-80.5665604569934,-2.32352748971546,
4.34291897104901));
#41282=CARTESIAN_POINT('Ctrl Pts',(-80.5270497572434,-3.04203951371433,
3.95850414531044));
#41283=CARTESIAN_POINT('Ctrl Pts',(-80.4875390574934,-3.66310933852919,
3.39195952885925));
#41284=CARTESIAN_POINT('Ctrl Pts',(-80.4480283577434,-4.11174419181654,
2.71169409882889));
#41285=CARTESIAN_POINT('Ctrl Pts',(-80.4085176579933,-4.56037904510389,
2.03142866879854));
#41286=CARTESIAN_POINT('Ctrl Pts',(-80.3690069582432,-4.83657892686373,
1.23744242518903));
#41287=CARTESIAN_POINT('Ctrl Pts',(-80.3294962584932,-4.90699332797998,
0.425607405622822));
#41288=CARTESIAN_POINT('Ctrl Pts',(-80.32261134763,-4.91926334289337,0.284141631017383));
#41289=CARTESIAN_POINT('Ctrl Pts',(-80.3157264367668,-4.92528476922512,
0.142133885922626));
#41290=CARTESIAN_POINT('Ctrl Pts',(-80.3088415259036,-4.92514409493932,
0.00011425152402452));
#41291=CARTESIAN_POINT('Origin',(-74.75,0.,0.));
#41292=CARTESIAN_POINT('',(-78.5911584740964,-4.92514886808152,-0.000113620830927696));
#41293=CARTESIAN_POINT('',(-78.8088415259036,-4.92515227384714,-0.000113155077916571));
#41294=CARTESIAN_POINT('',(-74.75,-4.925,-6.03138548580071E-16));
#41295=CARTESIAN_POINT('Ctrl Pts',(-78.5911584740964,-4.92514886808152,
-0.000113620830927696));
#41296=CARTESIAN_POINT('Ctrl Pts',(-78.6238604084024,-4.92448268450825,
0.674449036085999));
#41297=CARTESIAN_POINT('Ctrl Pts',(-78.6565623427083,-4.78477403277793,
1.3492791421555));
#41298=CARTESIAN_POINT('Ctrl Pts',(-78.6892642770142,-4.51534517405622,
1.96758304872409));
#41299=CARTESIAN_POINT('Ctrl Pts',(-78.7287749767642,-4.18981939196155,
2.71462203969505));
#41300=CARTESIAN_POINT('Ctrl Pts',(-78.7682856765143,-3.67493276089278,
3.37914613668745));
#41301=CARTESIAN_POINT('Ctrl Pts',(-78.8077963762643,-3.03285665751499,
3.88091556574396));
#41302=CARTESIAN_POINT('Ctrl Pts',(-78.8473070760143,-2.39078055413719,
4.38268499480047));
#41303=CARTESIAN_POINT('Ctrl Pts',(-78.8868177757644,-1.62151497845036,
4.72169975592108));
#41304=CARTESIAN_POINT('Ctrl Pts',(-78.9263284755144,-0.817947011417411,
4.85702458424017));
#41305=CARTESIAN_POINT('Ctrl Pts',(-78.9658391752644,-0.014379044384451,
4.99234941255926));
#41306=CARTESIAN_POINT('Ctrl Pts',(-79.0053498750145,0.823491313994628,
4.92398430807683));
#41307=CARTESIAN_POINT('Ctrl Pts',(-79.0448605747645,1.59449312272436,4.66018420284231));
#41308=CARTESIAN_POINT('Ctrl Pts',(-79.0843712745145,2.36549493145408,4.39638409760781));
#41309=CARTESIAN_POINT('Ctrl Pts',(-79.1238819742645,3.06962819053445,3.93714899162124));
#41310=CARTESIAN_POINT('Ctrl Pts',(-79.1633926740146,3.62187040442806,3.33793048168948));
#41311=CARTESIAN_POINT('Ctrl Pts',(-79.2029033737646,4.17411261832166,2.73871197175773));
#41312=CARTESIAN_POINT('Ctrl Pts',(-79.2424140735147,4.5744637870285,1.99951005788078));
#41313=CARTESIAN_POINT('Ctrl Pts',(-79.2819247732647,4.7745824161603,1.20958169434623));
#41314=CARTESIAN_POINT('Ctrl Pts',(-79.3214354730147,4.9747010452921,0.41965333081168));
#41315=CARTESIAN_POINT('Ctrl Pts',(-79.3609461727647,4.97458713484887,-0.421001482380465));
#41316=CARTESIAN_POINT('Ctrl Pts',(-79.4004568725147,4.77425443877746,-1.2108755838017));
#41317=CARTESIAN_POINT('Ctrl Pts',(-79.4399675722647,4.57392174270606,-2.00074968522294));
#41318=CARTESIAN_POINT('Ctrl Pts',(-79.4794782720148,4.17337026100648,-2.73984307487328));
#41319=CARTESIAN_POINT('Ctrl Pts',(-79.5189889717648,3.62096567661331,-3.33891190266436));
#41320=CARTESIAN_POINT('Ctrl Pts',(-79.5584996715148,3.06856109222011,-3.93798073045547));
#41321=CARTESIAN_POINT('Ctrl Pts',(-79.5980103712648,2.36430340513331,-4.39702499638732));
#41322=CARTESIAN_POINT('Ctrl Pts',(-79.6375210710149,1.59323013322142,-4.66061614679244));
#41323=CARTESIAN_POINT('Ctrl Pts',(-79.677031770765,0.822156861309541,-4.92420729719755));
#41324=CARTESIAN_POINT('Ctrl Pts',(-79.716542470515,-0.0157319954274157,
-4.99234533207592));
#41325=CARTESIAN_POINT('Ctrl Pts',(-79.756053170265,-0.819263258373394,
-4.85680273828705));
#41326=CARTESIAN_POINT('Ctrl Pts',(-79.7955638700151,-1.62279452131937,
-4.72126014449818));
#41327=CARTESIAN_POINT('Ctrl Pts',(-79.835074569765,-2.39196819047438,-4.38203692204205));
#41328=CARTESIAN_POINT('Ctrl Pts',(-79.8745852695151,-3.03390829031882,
-3.88009350545033));
#41329=CARTESIAN_POINT('Ctrl Pts',(-79.9140959692651,-3.67584839016326,
-3.37815008885861));
#41330=CARTESIAN_POINT('Ctrl Pts',(-79.9536066690152,-4.19055492069714,
-2.71348647813129));
#41331=CARTESIAN_POINT('Ctrl Pts',(-79.9931173687652,-4.51587823604353,
-1.96635929635804));
#41332=CARTESIAN_POINT('Ctrl Pts',(-80.025797737209,-4.78496194947119,-1.34839019611011));
#41333=CARTESIAN_POINT('Ctrl Pts',(-80.0584781056527,-4.92448119040597,
-0.674004538186427));
#41334=CARTESIAN_POINT('Ctrl Pts',(-80.0911584740964,-4.92514750914162,
0.000113799890342631));
#41335=CARTESIAN_POINT('Ctrl Pts',(-80.3088415259036,-4.92514409493932,
0.00011425152402452));
#41336=CARTESIAN_POINT('Ctrl Pts',(-80.2762157370168,-4.92447747635248,
-0.672879589897553));
#41337=CARTESIAN_POINT('Ctrl Pts',(-80.24358994813,-4.78543695671404,-1.34614041322281));
#41338=CARTESIAN_POINT('Ctrl Pts',(-80.2109641592432,-4.51722584013875,
-1.96326154491532));
#41339=CARTESIAN_POINT('Ctrl Pts',(-80.1714534594932,-4.19241503070861,
-2.71061168036438));
#41340=CARTESIAN_POINT('Ctrl Pts',(-80.1319427597431,-3.67816449137567,
-3.37562815573959));
#41341=CARTESIAN_POINT('Ctrl Pts',(-80.0924320599931,-3.03656880809882,
-3.87801174034342));
#41342=CARTESIAN_POINT('Ctrl Pts',(-80.052921360243,-2.39497312482196,-4.38039532494726));
#41343=CARTESIAN_POINT('Ctrl Pts',(-80.013410660493,-1.62603229760119,-4.72014601877972));
#41344=CARTESIAN_POINT('Ctrl Pts',(-79.9738999607429,-0.822594186851031,
-4.85623969634145));
#41345=CARTESIAN_POINT('Ctrl Pts',(-79.9343892609929,-0.0191560761008687,
-4.99233337390319));
#41346=CARTESIAN_POINT('Ctrl Pts',(-79.894878561243,0.818779318178687,-4.9247700351942));
#41347=CARTESIAN_POINT('Ctrl Pts',(-79.8553678614929,1.59003319812982,-4.66170780008762));
#41348=CARTESIAN_POINT('Ctrl Pts',(-79.8158571617429,2.36128707808095,-4.39864556498104));
#41349=CARTESIAN_POINT('Ctrl Pts',(-79.7763464619928,3.06585944370365,-3.94008443347687));
#41350=CARTESIAN_POINT('Ctrl Pts',(-79.7368357622428,3.61867478028739,-3.3413946218741));
#41351=CARTESIAN_POINT('Ctrl Pts',(-79.6973250624928,4.17149011687114,-2.74270481027132));
#41352=CARTESIAN_POINT('Ctrl Pts',(-79.6578143627428,4.57254842441591,-2.00388631856993));
#41353=CARTESIAN_POINT('Ctrl Pts',(-79.6183036629927,4.77342282216329,-1.2141498035192));
#41354=CARTESIAN_POINT('Ctrl Pts',(-79.5787929632427,4.97429721991067,-0.424413288468484));
#41355=CARTESIAN_POINT('Ctrl Pts',(-79.5392822634927,4.97498770786068,0.41624124993158));
#41356=CARTESIAN_POINT('Ctrl Pts',(-79.4997715637427,4.77541091114282,1.2063066833617));
#41357=CARTESIAN_POINT('Ctrl Pts',(-79.4602608639926,4.57583411442495,1.99637211679183));
#41358=CARTESIAN_POINT('Ctrl Pts',(-79.4207501642425,4.17599003303919,2.73584844525202));
#41359=CARTESIAN_POINT('Ctrl Pts',(-79.3812394644925,3.62415893273268,3.3354455796599));
#41360=CARTESIAN_POINT('Ctrl Pts',(-79.3417287647425,3.07232783242618,3.93504271406778));
#41361=CARTESIAN_POINT('Ctrl Pts',(-79.3022180649925,2.36850971319893,4.39476065442336));
#41362=CARTESIAN_POINT('Ctrl Pts',(-79.2627073652425,1.5976890161471,4.65908950247587));
#41363=CARTESIAN_POINT('Ctrl Pts',(-79.2231966654925,0.826868319095288,
4.92341835052838));
#41364=CARTESIAN_POINT('Ctrl Pts',(-79.1836859657424,-0.0109549557811001,
4.99235810627783));
#41365=CARTESIAN_POINT('Ctrl Pts',(-79.1441752659924,-0.814615548646616,
4.85758445042045));
#41366=CARTESIAN_POINT('Ctrl Pts',(-79.1046645662423,-1.61827614151215,
4.72281079456307));
#41367=CARTESIAN_POINT('Ctrl Pts',(-79.0651538664923,-2.38777405236682,
4.38432372709884));
#41368=CARTESIAN_POINT('Ctrl Pts',(-79.0256431667423,-3.0301941544924,3.88299479390851));
#41369=CARTESIAN_POINT('Ctrl Pts',(-78.9861324669923,-3.67261425661798,
3.38166586071818));
#41370=CARTESIAN_POINT('Ctrl Pts',(-78.9466217672422,-4.18795655001448,
2.71749506180175));
#41371=CARTESIAN_POINT('Ctrl Pts',(-78.9071110674922,-4.5139946213317,1.97067951353778));
#41372=CARTESIAN_POINT('Ctrl Pts',(-78.8743545536294,-4.78429787261529,
1.35152890333658));
#41373=CARTESIAN_POINT('Ctrl Pts',(-78.8415980397665,-4.92448647070407,
0.675573998008652));
#41374=CARTESIAN_POINT('Ctrl Pts',(-78.8088415259036,-4.92515227384714,
-0.000113155077916571));
#41375=CARTESIAN_POINT('Origin',(-74.75,0.,0.));
#41376=CARTESIAN_POINT('',(-77.0911584740964,-4.92453797299891,2.34045202216906E-5));
#41377=CARTESIAN_POINT('',(-77.3088415259036,-4.92459132837391,1.46844578195527E-5));
#41378=CARTESIAN_POINT('',(-74.75,-4.925,-6.03138548580071E-16));
#41379=CARTESIAN_POINT('Ctrl Pts',(-77.0911584740964,-4.9245376769549,2.34195166788631E-5));
#41380=CARTESIAN_POINT('Ctrl Pts',(-77.110221311652,-4.92460351006797,0.393366610892078));
#41381=CARTESIAN_POINT('Ctrl Pts',(-77.1292841492075,-4.87806963749634,
0.786699148933148));
#41382=CARTESIAN_POINT('Ctrl Pts',(-77.1483469867631,-4.78480271173096,
1.1686279851341));
#41383=CARTESIAN_POINT('Ctrl Pts',(-77.1878576865131,-4.59149248234959,
1.96023498115633));
#41384=CARTESIAN_POINT('Ctrl Pts',(-77.2273683862632,-4.1974216441505,2.702852793555));
#41385=CARTESIAN_POINT('Ctrl Pts',(-77.2668790860132,-3.65031620861451,
3.30678359219156));
#41386=CARTESIAN_POINT('Ctrl Pts',(-77.3063897857632,-3.10321077307853,
3.9107143908281));
#41387=CARTESIAN_POINT('Ctrl Pts',(-77.3459004855133,-2.40307074020566,
4.37595817570254));
#41388=CARTESIAN_POINT('Ctrl Pts',(-77.3854111852633,-1.63436550044067,
4.64635192368507));
#41389=CARTESIAN_POINT('Ctrl Pts',(-77.4249218850133,-0.865660260675676,
4.9167456716676));
#41390=CARTESIAN_POINT('Ctrl Pts',(-77.4644325847633,-0.0283898140185719,
4.99228938275823));
#41391=CARTESIAN_POINT('Ctrl Pts',(-77.5039432845133,0.776312113685768,
4.86385431998651));
#41392=CARTESIAN_POINT('Ctrl Pts',(-77.5434539842634,1.58101404139012,4.73541925721478));
#41393=CARTESIAN_POINT('Ctrl Pts',(-77.5829646840134,2.3531474501417,4.40300542058071));
#41394=CARTESIAN_POINT('Ctrl Pts',(-77.6224753837634,2.99949646977121,3.90675450502815));
#41395=CARTESIAN_POINT('Ctrl Pts',(-77.6619860835135,3.64584548940072,3.41050358947558));
#41396=CARTESIAN_POINT('Ctrl Pts',(-77.7014967832635,4.16641011990815,2.75041559500453));
#41397=CARTESIAN_POINT('Ctrl Pts',(-77.7410074830135,4.49832468022958,2.006192922343));
#41398=CARTESIAN_POINT('Ctrl Pts',(-77.7805181827635,4.83023924055099,1.2619702496815));
#41399=CARTESIAN_POINT('Ctrl Pts',(-77.8200288825136,4.9735037306864,0.433612898829542));
#41400=CARTESIAN_POINT('Ctrl Pts',(-77.8595395822637,4.91082359979706,-0.378856001820336));
#41401=CARTESIAN_POINT('Ctrl Pts',(-77.8990502820137,4.84814346890771,-1.19132490247023));
#41402=CARTESIAN_POINT('Ctrl Pts',(-77.9385609817636,4.57951871699359,-1.98790535291803));
#41403=CARTESIAN_POINT('Ctrl Pts',(-77.9780716815137,4.13738303272748,-2.67241249674817));
#41404=CARTESIAN_POINT('Ctrl Pts',(-78.0175823812637,3.69524734846136,-3.35691964057832));
#41405=CARTESIAN_POINT('Ctrl Pts',(-78.0570930810138,3.07960073184324,-3.92935347779079));
#41406=CARTESIAN_POINT('Ctrl Pts',(-78.0966037807638,2.36478217805084,-4.32059370978506));
#41407=CARTESIAN_POINT('Ctrl Pts',(-78.1361144805139,1.64996362425846,-4.71183394177931));
#41408=CARTESIAN_POINT('Ctrl Pts',(-78.1756251802638,0.835973133291798,
-4.92188056855537));
#41409=CARTESIAN_POINT('Ctrl Pts',(-78.2151358800138,0.0210976824875499,
-4.92537104143333));
#41410=CARTESIAN_POINT('Ctrl Pts',(-78.2546465797639,-0.793777768316698,
-4.92886151431129));
#41411=CARTESIAN_POINT('Ctrl Pts',(-78.2941572795139,-1.60953817895853,
-4.72579583329114));
#41412=CARTESIAN_POINT('Ctrl Pts',(-78.333667979264,-2.32768206849062,-4.34069366654293));
#41413=CARTESIAN_POINT('Ctrl Pts',(-78.373178679014,-3.04582595802271,-3.95559149979471));
#41414=CARTESIAN_POINT('Ctrl Pts',(-78.412689378764,-3.66635332644505,-3.38845284731842));
#41415=CARTESIAN_POINT('Ctrl Pts',(-78.452200078514,-4.11433703191033,-2.70775844063091));
#41416=CARTESIAN_POINT('Ctrl Pts',(-78.4917107782641,-4.56232073737562,
-2.02706403394338));
#41417=CARTESIAN_POINT('Ctrl Pts',(-78.5312214780141,-4.83776077988383,
-1.23281387304462));
#41418=CARTESIAN_POINT('Ctrl Pts',(-78.5707321777641,-4.90739833457764,
-0.420911850120484));
#41419=CARTESIAN_POINT('Ctrl Pts',(-78.5775409432082,-4.91939877443344,
-0.280999105657526));
#41420=CARTESIAN_POINT('Ctrl Pts',(-78.5843497086523,-4.92528757203862,
-0.140562160214772));
#41421=CARTESIAN_POINT('Ctrl Pts',(-78.5911584740964,-4.92514886808152,
-0.000113620830927696));
#41422=CARTESIAN_POINT('Ctrl Pts',(-78.8088415259036,-4.92515227384714,
-0.000113155077916571));
#41423=CARTESIAN_POINT('Ctrl Pts',(-78.8020873400165,-4.92528955824227,
-0.139435570540877));
#41424=CARTESIAN_POINT('Ctrl Pts',(-78.7953331541293,-4.91949491513351,
-0.278746602294923));
#41425=CARTESIAN_POINT('Ctrl Pts',(-78.7885789682421,-4.90768586809107,
-0.417545928509096));
#41426=CARTESIAN_POINT('Ctrl Pts',(-78.7490682684921,-4.83860519429525,
-1.22949552468054));
#41427=CARTESIAN_POINT('Ctrl Pts',(-78.7095575687421,-4.56370999746566,
-2.02393441941193));
#41428=CARTESIAN_POINT('Ctrl Pts',(-78.670046868992,-4.11619324668281,-2.704935921754));
#41429=CARTESIAN_POINT('Ctrl Pts',(-78.630536169242,-3.66867649589997,-3.38593742409605));
#41430=CARTESIAN_POINT('Ctrl Pts',(-78.591025469492,-3.04853819116387,-3.9535015340488));
#41431=CARTESIAN_POINT('Ctrl Pts',(-78.551514769742,-2.33065863049451,-4.33909616636603));
#41432=CARTESIAN_POINT('Ctrl Pts',(-78.5120040699919,-1.61277906982514,
-4.72469079868326));
#41433=CARTESIAN_POINT('Ctrl Pts',(-78.4724933702418,-0.797158253222491,
-4.92831595336498));
#41434=CARTESIAN_POINT('Ctrl Pts',(-78.4329826704918,0.0177194653744605,
-4.92538436820628));
#41435=CARTESIAN_POINT('Ctrl Pts',(-78.3934719707418,0.832597183971412,
-4.92245278304758));
#41436=CARTESIAN_POINT('Ctrl Pts',(-78.3539612709918,1.64673180456268,-4.71296445804845));
#41437=CARTESIAN_POINT('Ctrl Pts',(-78.3144505712418,2.36181840000114,-4.32221460647475));
#41438=CARTESIAN_POINT('Ctrl Pts',(-78.2749398714918,3.0769049954396,-3.93146475490105));
#41439=CARTESIAN_POINT('Ctrl Pts',(-78.2354291717417,3.69294356572525,-3.35945337675278));
#41440=CARTESIAN_POINT('Ctrl Pts',(-78.1959184719917,4.13554888877892,-2.67524960205178));
#41441=CARTESIAN_POINT('Ctrl Pts',(-78.1564077722416,4.57815421183259,-1.9910458273508));
#41442=CARTESIAN_POINT('Ctrl Pts',(-78.1168970724916,4.84732628765426,-1.1946496560971));
#41443=CARTESIAN_POINT('Ctrl Pts',(-78.0773863727416,4.91056312282638,-0.382224010811509));
#41444=CARTESIAN_POINT('Ctrl Pts',(-78.0378756729916,4.9737999579985,0.430201634474102));
#41445=CARTESIAN_POINT('Ctrl Pts',(-77.9983649732415,4.83110155252106,1.2586567537916));
#41446=CARTESIAN_POINT('Ctrl Pts',(-77.9588542734915,4.49969856804995,2.00310705263756));
#41447=CARTESIAN_POINT('Ctrl Pts',(-77.9193435737415,4.16829558357886,2.74755735148348));
#41448=CARTESIAN_POINT('Ctrl Pts',(-77.8798328739914,3.6481880201141,3.40800282985787));
#41449=CARTESIAN_POINT('Ctrl Pts',(-77.8403221742414,3.00217737795472,3.90469663436248));
#41450=CARTESIAN_POINT('Ctrl Pts',(-77.8008114744914,2.35616673579532,4.40139043886709));
#41451=CARTESIAN_POINT('Ctrl Pts',(-77.7613007747414,1.58425301494129,4.73433256950191));
#41452=CARTESIAN_POINT('Ctrl Pts',(-77.7217900749914,0.779643666424622,
4.86332013350593));
#41453=CARTESIAN_POINT('Ctrl Pts',(-77.6822793752413,-0.0249656820920473,
4.99230769750994));
#41454=CARTESIAN_POINT('Ctrl Pts',(-77.6427686754913,-0.86227065827136,
4.91734069488313));
#41455=CARTESIAN_POINT('Ctrl Pts',(-77.6032579757413,-1.6311698355519,4.64747300536884));
#41456=CARTESIAN_POINT('Ctrl Pts',(-77.5637472759912,-2.40006901283244,
4.37760531585456));
#41457=CARTESIAN_POINT('Ctrl Pts',(-77.5242365762412,-3.10056239121421,
3.91283693945278));
#41458=CARTESIAN_POINT('Ctrl Pts',(-77.4847258764912,-3.64806446717552,
3.30928400931355));
#41459=CARTESIAN_POINT('Ctrl Pts',(-77.4452151767411,-4.19556654313682,
2.70573107917432));
#41460=CARTESIAN_POINT('Ctrl Pts',(-77.4057044769911,-4.59007731667766,
1.96339359529763));
#41461=CARTESIAN_POINT('Ctrl Pts',(-77.3661937772411,-4.78396557727188,
1.17191436367405));
#41462=CARTESIAN_POINT('Ctrl Pts',(-77.3470763601286,-4.87777922204265,
0.788953831399374));
#41463=CARTESIAN_POINT('Ctrl Pts',(-77.3279589430161,-4.92462415434814,
0.394488485502017));
#41464=CARTESIAN_POINT('Ctrl Pts',(-77.3088415259036,-4.92459132837391,
1.46844578195527E-5));
#41465=CARTESIAN_POINT('Origin',(-74.75,0.,0.));
#41466=CARTESIAN_POINT('',(-75.5911584740964,-4.93145818296612,0.00170945267300153));
#41467=CARTESIAN_POINT('',(-75.8088415259036,-4.93185981856261,0.00388372659001099));
#41468=CARTESIAN_POINT('',(-74.75,-4.925,-6.03138548580071E-16));
#41469=CARTESIAN_POINT('Ctrl Pts',(-75.5911584740964,-4.93145818296612,
0.00170945267300153));
#41470=CARTESIAN_POINT('Ctrl Pts',(-75.5965822149016,-4.93204081057214,
0.113167419548451));
#41471=CARTESIAN_POINT('Ctrl Pts',(-75.6020059557068,-4.92860871675615,
0.224592305800187));
#41472=CARTESIAN_POINT('Ctrl Pts',(-75.607429696512,-4.92105000563757,0.335738029486276));
#41473=CARTESIAN_POINT('Ctrl Pts',(-75.686451096012,-4.810923074344,1.95507990985986));
#41474=CARTESIAN_POINT('Ctrl Pts',(-75.7654724955121,-3.82483311757502,
3.51516354851337));
#41475=CARTESIAN_POINT('Ctrl Pts',(-75.8444938950122,-2.40735607849465,
4.30649291473166));
#41476=CARTESIAN_POINT('Ctrl Pts',(-75.9235152945122,-0.989879039414278,
5.09782228094995));
#41477=CARTESIAN_POINT('Ctrl Pts',(-76.0025366940123,0.85898508197749,5.12039737473303));
#41478=CARTESIAN_POINT('Ctrl Pts',(-76.0815580935123,2.29413116832581,4.36708108920334));
#41479=CARTESIAN_POINT('Ctrl Pts',(-76.1605794930124,3.72927725467414,3.61376480367365));
#41480=CARTESIAN_POINT('Ctrl Pts',(-76.2396008925124,4.75070530597902,2.08455713883121));
#41481=CARTESIAN_POINT('Ctrl Pts',(-76.3186222920125,4.90865109371366,0.464760615946058));
#41482=CARTESIAN_POINT('Ctrl Pts',(-76.3581329917625,4.98762398758099,-0.345137645496505));
#41483=CARTESIAN_POINT('Ctrl Pts',(-76.3976436915125,4.85072631555575,-1.17768312144974));
#41484=CARTESIAN_POINT('Ctrl Pts',(-76.4371543912626,4.52998832978331,-1.92803440327652));
#41485=CARTESIAN_POINT('Ctrl Pts',(-76.4766650910126,4.20925034401087,-2.6783856851033));
#41486=CARTESIAN_POINT('Ctrl Pts',(-76.5161757907626,3.70467204449123,-3.34654277280362));
#41487=CARTESIAN_POINT('Ctrl Pts',(-76.5556864905126,3.06815643951909,-3.85374200240443));
#41488=CARTESIAN_POINT('Ctrl Pts',(-76.5951971902627,2.43164083454696,-4.36094123200524));
#41489=CARTESIAN_POINT('Ctrl Pts',(-76.6347078900127,1.66318792412234,-4.70718260350654));
#41490=CARTESIAN_POINT('Ctrl Pts',(-76.6742185897627,0.86029094445069,-4.84971500783713));
#41491=CARTESIAN_POINT('Ctrl Pts',(-76.7137292895128,0.0573939647790152,
-4.99224741216772));
#41492=CARTESIAN_POINT('Ctrl Pts',(-76.7532399892629,-0.779947084139697,
-4.93107084932759));
#41493=CARTESIAN_POINT('Ctrl Pts',(-76.7927506890129,-1.5529731345604,-4.67403983231761));
#41494=CARTESIAN_POINT('Ctrl Pts',(-76.8322613887629,-2.3259991849811,-4.41700881530763));
#41495=CARTESIAN_POINT('Ctrl Pts',(-76.8717720885129,-3.03471023690379,
-3.96412334412782));
#41496=CARTESIAN_POINT('Ctrl Pts',(-76.9112827882629,-3.59236424510066,
-3.36983619140984));
#41497=CARTESIAN_POINT('Ctrl Pts',(-76.9507934880129,-4.15001825329752,
-2.77554903869188));
#41498=CARTESIAN_POINT('Ctrl Pts',(-76.990304187763,-4.55661521776857,-2.03986020443576));
#41499=CARTESIAN_POINT('Ctrl Pts',(-77.029814887513,-4.76363888972227,-1.25171769748482));
#41500=CARTESIAN_POINT('Ctrl Pts',(-77.0502627497075,-4.87077927300793,
-0.843832505025608));
#41501=CARTESIAN_POINT('Ctrl Pts',(-77.070710611902,-4.92446706068804,-0.421898413942657));
#41502=CARTESIAN_POINT('Ctrl Pts',(-77.0911584740964,-4.9245376769549,2.34195166788631E-5));
#41503=CARTESIAN_POINT('Ctrl Pts',(-77.3088415259036,-4.92459132837391,
1.46844578195527E-5));
#41504=CARTESIAN_POINT('Ctrl Pts',(-77.2884482432661,-4.9245563116472,-0.420785660613278));
#41505=CARTESIAN_POINT('Ctrl Pts',(-77.2680549606285,-4.87117765087757,
-0.841595627056218));
#41506=CARTESIAN_POINT('Ctrl Pts',(-77.247661677991,-4.76456575302619,-1.24846007914821));
#41507=CARTESIAN_POINT('Ctrl Pts',(-77.208150978241,-4.55801192053866,-2.03673431097644));
#41508=CARTESIAN_POINT('Ctrl Pts',(-77.1686402784909,-4.15163850791598,
-2.77266179526241));
#41509=CARTESIAN_POINT('Ctrl Pts',(-77.1291295787409,-3.59453475390508,
-3.36735158860536));
#41510=CARTESIAN_POINT('Ctrl Pts',(-77.0896188789909,-3.03743099989419,
-3.96204138194831));
#41511=CARTESIAN_POINT('Ctrl Pts',(-77.0501081792409,-2.32959690449509,
-4.41549348434824));
#41512=CARTESIAN_POINT('Ctrl Pts',(-77.0105974794909,-1.55646039394619,
-4.6730137396139));
#41513=CARTESIAN_POINT('Ctrl Pts',(-76.9710867797408,-0.783323883397288,
-4.93053399487957));
#41514=CARTESIAN_POINT('Ctrl Pts',(-76.9315760799908,0.055115042301422,
-4.99212240301097));
#41515=CARTESIAN_POINT('Ctrl Pts',(-76.8920653802408,0.857533325507661,
-4.85022314878024));
#41516=CARTESIAN_POINT('Ctrl Pts',(-76.8525546804907,1.65995160871392,-4.70832389454951));
#41517=CARTESIAN_POINT('Ctrl Pts',(-76.8130439807407,2.42634924942772,-4.36293697795663));
#41518=CARTESIAN_POINT('Ctrl Pts',(-76.7735332809906,3.06435357769784,-3.85600708998388));
#41519=CARTESIAN_POINT('Ctrl Pts',(-76.7340225812406,3.70235790596796,-3.34907720201115));
#41520=CARTESIAN_POINT('Ctrl Pts',(-76.6945118814906,4.21196892179439,-2.68060434265857));
#41521=CARTESIAN_POINT('Ctrl Pts',(-76.6550011817406,4.53131364928107,-1.9308216777245));
#41522=CARTESIAN_POINT('Ctrl Pts',(-76.6154904819906,4.85065837676774,-1.18103901279044));
#41523=CARTESIAN_POINT('Ctrl Pts',(-76.5759797822405,4.97973681591463,-0.349946542274868));
#41524=CARTESIAN_POINT('Ctrl Pts',(-76.5364690824904,4.90364501449345,0.461129615068031));
#41525=CARTESIAN_POINT('Ctrl Pts',(-76.4969583827404,4.82755321307227,1.27220577241095));
#41526=CARTESIAN_POINT('Ctrl Pts',(-76.4574476829904,4.54629117108303,2.06326561658121));
#41527=CARTESIAN_POINT('Ctrl Pts',(-76.4179369832404,4.09244767227833,2.74074969716858));
#41528=CARTESIAN_POINT('Ctrl Pts',(-76.3784262834904,3.63860417347364,3.41823377775594));
#41529=CARTESIAN_POINT('Ctrl Pts',(-76.3389155837403,3.01217921785349,3.9821420947604));
#41530=CARTESIAN_POINT('Ctrl Pts',(-76.2994048839903,2.29156928683899,4.36046055554361));
#41531=CARTESIAN_POINT('Ctrl Pts',(-76.2598941842403,1.57095935582447,4.73877901632683));
#41532=CARTESIAN_POINT('Ctrl Pts',(-76.2203834844902,0.756164449415575,
4.9315076208888));
#41533=CARTESIAN_POINT('Ctrl Pts',(-76.1808727847402,-0.059816786502471,
4.92285971725886));
#41534=CARTESIAN_POINT('Ctrl Pts',(-76.1413620849902,-0.875798022420494,
4.91421181362892));
#41535=CARTESIAN_POINT('Ctrl Pts',(-76.1018513852402,-1.69296558784768,
4.70418740180709));
#41536=CARTESIAN_POINT('Ctrl Pts',(-76.0623406854901,-2.40245776805243,
4.30569922684081));
#41537=CARTESIAN_POINT('Ctrl Pts',(-75.9833192859901,-3.82144212846192,
3.50872287690825));
#41538=CARTESIAN_POINT('Ctrl Pts',(-75.90429788649,-4.80972494798167,1.9578914743979));
#41539=CARTESIAN_POINT('Ctrl Pts',(-75.8252764869899,-4.92120160549743,
0.340887420253297));
#41540=CARTESIAN_POINT('Ctrl Pts',(-75.8197981666278,-4.92892995309229,
0.228785302453847));
#41541=CARTESIAN_POINT('Ctrl Pts',(-75.8143198462657,-4.93244416019434,
0.116365143036017));
#41542=CARTESIAN_POINT('Ctrl Pts',(-75.8088415259036,-4.93185981856261,
0.00388372659001099));
#41543=CARTESIAN_POINT('Origin',(-74.75,0.,0.));
#41544=CARTESIAN_POINT('',(-74.0911584740964,-4.91843222427485,0.00245724012685411));
#41545=CARTESIAN_POINT('',(-74.3088415259036,-4.91847745023605,0.00259239093822753));
#41546=CARTESIAN_POINT('',(-74.75,-4.925,-6.03138548580071E-16));
#41547=CARTESIAN_POINT('Ctrl Pts',(-74.0911584740964,-4.91843222427485,
0.00245724012685411));
#41548=CARTESIAN_POINT('Ctrl Pts',(-74.1224538179012,-4.92156279260847,
0.650146294184244));
#41549=CARTESIAN_POINT('Ctrl Pts',(-74.153749161706,-4.80268279810373,1.29675391287114));
#41550=CARTESIAN_POINT('Ctrl Pts',(-74.1850445055109,-4.55640455625903,
1.89046313642067));
#41551=CARTESIAN_POINT('Ctrl Pts',(-74.264065905011,-3.93454683012746,3.3895913784221));
#41552=CARTESIAN_POINT('Ctrl Pts',(-74.3430873045111,-2.50043215929785,
4.55145368693655));
#41553=CARTESIAN_POINT('Ctrl Pts',(-74.4221087040112,-0.905034099899794,
4.84914491655614));
#41554=CARTESIAN_POINT('Ctrl Pts',(-74.5011301035112,0.690363959498285,
5.14683614617574));
#41555=CARTESIAN_POINT('Ctrl Pts',(-74.5801515030112,2.4470454074648,4.58035629690046));
#41556=CARTESIAN_POINT('Ctrl Pts',(-74.6591729025113,3.56776108938243,3.40663242401753));
#41557=CARTESIAN_POINT('Ctrl Pts',(-74.7381943020113,4.68847677130004,2.23290855113462));
#41558=CARTESIAN_POINT('Ctrl Pts',(-74.8172157015114,5.17322668716877,0.451940654644055));
#41559=CARTESIAN_POINT('Ctrl Pts',(-74.8962371010115,4.80217577389113,-1.12800752674652));
#41560=CARTESIAN_POINT('Ctrl Pts',(-74.9752585005115,4.43112486061349,-2.70795570813711));
#41561=CARTESIAN_POINT('Ctrl Pts',(-75.0542799000116,3.2042731181895,-4.08688417442772));
#41562=CARTESIAN_POINT('Ctrl Pts',(-75.1333012995116,1.67802622625532,-4.63884698329907));
#41563=CARTESIAN_POINT('Ctrl Pts',(-75.2123226990117,0.151779334321143,
-5.19080979217042));
#41564=CARTESIAN_POINT('Ctrl Pts',(-75.2913440985118,-1.6738627071232,-4.91580694362251));
#41565=CARTESIAN_POINT('Ctrl Pts',(-75.3703654980118,-2.96960177493628,
-3.93900545830171));
#41566=CARTESIAN_POINT('Ctrl Pts',(-75.4439631567067,-4.17640603648892,
-3.02924806620143));
#41567=CARTESIAN_POINT('Ctrl Pts',(-75.5175608154016,-4.92355219533978,
-1.51072369993773));
#41568=CARTESIAN_POINT('Ctrl Pts',(-75.5911584740964,-4.93145818296612,
0.00170945267300153));
#41569=CARTESIAN_POINT('Ctrl Pts',(-75.8088415259036,-4.93185981856261,
0.00388372659001099));
#41570=CARTESIAN_POINT('Ctrl Pts',(-75.7352984467657,-4.92401539179933,
-1.50611006063952));
#41571=CARTESIAN_POINT('Ctrl Pts',(-75.6617553676277,-4.1775546932613,-3.02714322807678));
#41572=CARTESIAN_POINT('Ctrl Pts',(-75.5882122884898,-2.97212463234744,
-3.93798622059295));
#41573=CARTESIAN_POINT('Ctrl Pts',(-75.5091908889897,-1.67690050616995,
-4.91667910151568));
#41574=CARTESIAN_POINT('Ctrl Pts',(-75.4301694894897,0.148218241696821,
-5.19088815758227));
#41575=CARTESIAN_POINT('Ctrl Pts',(-75.3511480899896,1.67475699940288,-4.63946497019405));
#41576=CARTESIAN_POINT('Ctrl Pts',(-75.2721266904895,3.20129575710896,-4.08804178280584));
#41577=CARTESIAN_POINT('Ctrl Pts',(-75.1931052909895,4.42925452465434,-2.71098635196282));
#41578=CARTESIAN_POINT('Ctrl Pts',(-75.1140838914894,4.80143977898294,-1.13156518854111));
#41579=CARTESIAN_POINT('Ctrl Pts',(-75.0350624919894,5.17362503331154,0.447855974880574));
#41580=CARTESIAN_POINT('Ctrl Pts',(-74.9560410924893,4.69003677442338,2.22964287088094));
#41581=CARTESIAN_POINT('Ctrl Pts',(-74.8770196929893,3.57008894292872,3.4042977373349));
#41582=CARTESIAN_POINT('Ctrl Pts',(-74.7979982934892,2.45014111143405,4.57895260378886));
#41583=CARTESIAN_POINT('Ctrl Pts',(-74.7189768939892,0.693833707332852,
5.14647544069641));
#41584=CARTESIAN_POINT('Ctrl Pts',(-74.6399554944891,-0.90172743084978,
4.84975223650184));
#41585=CARTESIAN_POINT('Ctrl Pts',(-74.560934094989,-2.49728856903242,4.55302903230727));
#41586=CARTESIAN_POINT('Ctrl Pts',(-74.4819126954889,-3.93210344129651,
3.3920597870106));
#41587=CARTESIAN_POINT('Ctrl Pts',(-74.4028912959889,-4.55505162183579,
1.89350503658887));
#41588=CARTESIAN_POINT('Ctrl Pts',(-74.3715413726271,-4.80219198940474,
1.29898789469625));
#41589=CARTESIAN_POINT('Ctrl Pts',(-74.3401914492653,-4.92155077598789,
0.651337387434103));
#41590=CARTESIAN_POINT('Ctrl Pts',(-74.3088415259036,-4.91847745023605,
0.00259239093822753));
#41591=CARTESIAN_POINT('Origin',(-74.75,0.,0.));
#41592=CARTESIAN_POINT('',(-72.5911584740964,-4.92473478262889,-0.000479420352050008));
#41593=CARTESIAN_POINT('',(-72.8088415259036,-4.92403075528272,-0.00394394407346908));
#41594=CARTESIAN_POINT('',(-74.75,-4.925,-6.03138548580071E-16));
#41595=CARTESIAN_POINT('Ctrl Pts',(-72.5911584740964,-4.92473478262889,
-0.000479420352050008));
#41596=CARTESIAN_POINT('Ctrl Pts',(-72.6088147211509,-4.92488354658816,
0.363652102799084));
#41597=CARTESIAN_POINT('Ctrl Pts',(-72.6264709682053,-4.88500686021711,
0.727870072460014));
#41598=CARTESIAN_POINT('Ctrl Pts',(-72.6441272152598,-4.80481154670615,
1.08333843603181));
#41599=CARTESIAN_POINT('Ctrl Pts',(-72.6836379150098,-4.62535251763178,
1.87879648214977));
#41600=CARTESIAN_POINT('Ctrl Pts',(-72.7231486147599,-4.24399252838692,
2.63043969636934));
#41601=CARTESIAN_POINT('Ctrl Pts',(-72.7626593145099,-3.70793942458222,
3.24285315456735));
#41602=CARTESIAN_POINT('Ctrl Pts',(-72.8021700142599,-3.17188632077752,
3.85526661276537));
#41603=CARTESIAN_POINT('Ctrl Pts',(-72.8416807140099,-2.481140102413,4.32845031494182));
#41604=CARTESIAN_POINT('Ctrl Pts',(-72.88119141376,-1.71677733901996,4.61419402457444));
#41605=CARTESIAN_POINT('Ctrl Pts',(-72.92070211351,-0.952414575626897,4.89993773420706));
#41606=CARTESIAN_POINT('Ctrl Pts',(-72.96021281326,-0.11443526720532,4.99824145129583));
#41607=CARTESIAN_POINT('Ctrl Pts',(-72.9997235130101,0.690951841327282,
4.8819507927587));
#41608=CARTESIAN_POINT('Ctrl Pts',(-73.0787449125101,2.30172605839249,4.64936947568446));
#41609=CARTESIAN_POINT('Ctrl Pts',(-73.1577663120102,3.78213147590179,3.55841065610665));
#41610=CARTESIAN_POINT('Ctrl Pts',(-73.2367877115102,4.46836735735957,2.09000675043046));
#41611=CARTESIAN_POINT('Ctrl Pts',(-73.3158091110103,5.15460323881732,0.621602844754309));
#41612=CARTESIAN_POINT('Ctrl Pts',(-73.3948305105104,5.0466695842236,-1.2242461470202));
#41613=CARTESIAN_POINT('Ctrl Pts',(-73.4738519100104,4.19072380063174,-2.603666364978));
#41614=CARTESIAN_POINT('Ctrl Pts',(-73.5528733095105,3.33477801703989,-3.98308658293581));
#41615=CARTESIAN_POINT('Ctrl Pts',(-73.6318947090105,1.73082010444989,-4.8960780270769));
#41616=CARTESIAN_POINT('Ctrl Pts',(-73.7109161085106,0.10812014196865,-4.93130441337073));
#41617=CARTESIAN_POINT('Ctrl Pts',(-73.7899375080106,-1.51457982051261,
-4.96653079966455));
#41618=CARTESIAN_POINT('Ctrl Pts',(-73.8689589075107,-3.15602183288511,
-4.12399212811109));
#41619=CARTESIAN_POINT('Ctrl Pts',(-73.9479803070108,-4.07194244835461,
-2.78452570459015));
#41620=CARTESIAN_POINT('Ctrl Pts',(-73.995706362706,-4.62512523912847,-1.97553662650135));
#41621=CARTESIAN_POINT('Ctrl Pts',(-74.0434324184012,-4.91365804190512,
-0.985282152029947));
#41622=CARTESIAN_POINT('Ctrl Pts',(-74.0911584740964,-4.91843222427485,
0.00245724012685411));
#41623=CARTESIAN_POINT('Ctrl Pts',(-74.3088415259036,-4.91847745023605,
0.00259239093822753));
#41624=CARTESIAN_POINT('Ctrl Pts',(-74.2611700497653,-4.91380407436992,
-0.983905447139712));
#41625=CARTESIAN_POINT('Ctrl Pts',(-74.213498573627,-4.62603089007891,-1.97293407298634));
#41626=CARTESIAN_POINT('Ctrl Pts',(-74.1658270974888,-4.07396738632402,
-2.78151743232188));
#41627=CARTESIAN_POINT('Ctrl Pts',(-74.0868056979887,-3.15885348145848,
-4.12184489526421));
#41628=CARTESIAN_POINT('Ctrl Pts',(-74.0077842984886,-1.51754418291289,
-4.96635956560206));
#41629=CARTESIAN_POINT('Ctrl Pts',(-73.9287628989886,0.104965517004485,
-4.93181901953187));
#41630=CARTESIAN_POINT('Ctrl Pts',(-73.8497414994885,1.72747521692181,-4.89727847346167));
#41631=CARTESIAN_POINT('Ctrl Pts',(-73.7707200999884,3.33118531821094,-3.98368271098348));
#41632=CARTESIAN_POINT('Ctrl Pts',(-73.6916987004883,4.18850610344658,-2.60569102857425));
#41633=CARTESIAN_POINT('Ctrl Pts',(-73.6126773009883,5.04582688868223,-1.227699346165));
#41634=CARTESIAN_POINT('Ctrl Pts',(-73.5336559014883,5.1567583578644,0.614688256175252));
#41635=CARTESIAN_POINT('Ctrl Pts',(-73.4546345019882,4.47052726991194,2.08546495386977));
#41636=CARTESIAN_POINT('Ctrl Pts',(-73.3756131024882,3.78429618195948,3.55624165156429));
#41637=CARTESIAN_POINT('Ctrl Pts',(-73.2965917029881,2.30090253687238,4.65540744461303));
#41638=CARTESIAN_POINT('Ctrl Pts',(-73.217570303488,0.69438387466605,4.88386064110368));
#41639=CARTESIAN_POINT('Ctrl Pts',(-73.138548903988,-0.912134787540277,
5.11231383759433));
#41640=CARTESIAN_POINT('Ctrl Pts',(-73.0595275044879,-2.64177846686585,
4.47005443752691));
#41641=CARTESIAN_POINT('Ctrl Pts',(-72.9805061049879,-3.71118316350073,
3.24908690921855));
#41642=CARTESIAN_POINT('Ctrl Pts',(-72.9232845786265,-4.48556794315112,
2.36495139593291));
#41643=CARTESIAN_POINT('Ctrl Pts',(-72.866063052265,-4.91374989924659,1.1773645668908));
#41644=CARTESIAN_POINT('Ctrl Pts',(-72.8088415259036,-4.92403075528272,
-0.00394394407346908));
#41645=CARTESIAN_POINT('Origin',(-74.75,0.,0.));
#41646=CARTESIAN_POINT('',(-71.0911584740964,-4.92530702679097,7.89345770752653E-5));
#41647=CARTESIAN_POINT('',(-71.3088415259036,-4.92529298732208,6.25886409129966E-5));
#41648=CARTESIAN_POINT('',(-74.75,-4.925,-6.03138548580071E-16));
#41649=CARTESIAN_POINT('Ctrl Pts',(-71.0911584740964,-4.92530702679097,
7.89345770752653E-5));
#41650=CARTESIAN_POINT('Ctrl Pts',(-71.0951756244005,-4.92537049355805,
0.0829354331087285));
#41651=CARTESIAN_POINT('Ctrl Pts',(-71.0991927747046,-4.92332239207377,
0.165788792394246));
#41652=CARTESIAN_POINT('Ctrl Pts',(-71.1032099250087,-4.91914176021086,
0.248534405960264));
#41653=CARTESIAN_POINT('Ctrl Pts',(-71.1427206247587,-4.87802313685915,
1.06237925759848));
#41654=CARTESIAN_POINT('Ctrl Pts',(-71.1822313245088,-4.63060960650741,
1.86580109561577));
#41655=CARTESIAN_POINT('Ctrl Pts',(-71.2217420242588,-4.20677566240803,
2.56178907813124));
#41656=CARTESIAN_POINT('Ctrl Pts',(-71.2612527240088,-3.78294171830867,
3.2577770606467));
#41657=CARTESIAN_POINT('Ctrl Pts',(-71.3007634237588,-3.18268736046168,
3.84633118766033));
#41658=CARTESIAN_POINT('Ctrl Pts',(-71.3402741235088,-2.47849220107993,
4.25638383154797));
#41659=CARTESIAN_POINT('Ctrl Pts',(-71.3797848232589,-1.77429704169817,
4.6664364754356));
#41660=CARTESIAN_POINT('Ctrl Pts',(-71.4192955230089,-0.966161080781646,
4.89798763619723));
#41661=CARTESIAN_POINT('Ctrl Pts',(-71.458806222759,-0.15166437801373,4.92308015523622));
#41662=CARTESIAN_POINT('Ctrl Pts',(-71.498316922509,0.662832324754209,4.94817267427521));
#41663=CARTESIAN_POINT('Ctrl Pts',(-71.537827622259,1.48368976937354,4.76680655159155));
#41664=CARTESIAN_POINT('Ctrl Pts',(-71.577338322009,2.21179022592752,4.40087706791648));
#41665=CARTESIAN_POINT('Ctrl Pts',(-71.616849021759,2.93989068248148,4.03494758424142));
#41666=CARTESIAN_POINT('Ctrl Pts',(-71.6563597215091,3.57523415097011,3.48445473957497));
#41667=CARTESIAN_POINT('Ctrl Pts',(-71.6958704212591,4.04110647518502,2.81587788992091));
#41668=CARTESIAN_POINT('Ctrl Pts',(-71.7353811210091,4.50697879939993,2.14730104026684));
#41669=CARTESIAN_POINT('Ctrl Pts',(-71.7748918207592,4.80337997934113,1.36064018562517));
#41670=CARTESIAN_POINT('Ctrl Pts',(-71.8144025205092,4.89451596279089,0.550865531588069));
#41671=CARTESIAN_POINT('Ctrl Pts',(-71.8539132202592,4.98565194624065,-0.258909122449052));
#41672=CARTESIAN_POINT('Ctrl Pts',(-71.8934239200093,4.87152273319896,-1.09179757588159));
#41673=CARTESIAN_POINT('Ctrl Pts',(-71.9329346197593,4.56591779143395,-1.84719557969087));
#41674=CARTESIAN_POINT('Ctrl Pts',(-71.9724453195093,4.26031284966897,-2.6025935835001));
#41675=CARTESIAN_POINT('Ctrl Pts',(-72.0119560192594,3.76323217918069,-3.28050113768607));
#41676=CARTESIAN_POINT('Ctrl Pts',(-72.0514667190094,3.13467977422752,-3.79913264594829));
#41677=CARTESIAN_POINT('Ctrl Pts',(-72.0909774187594,2.50612736927432,-4.31776415421053));
#41678=CARTESIAN_POINT('Ctrl Pts',(-72.1304881185094,1.74610322985622,-4.677119616549));
#41679=CARTESIAN_POINT('Ctrl Pts',(-72.1699988182594,0.946413527352501,
-4.83366628896438));
#41680=CARTESIAN_POINT('Ctrl Pts',(-72.2095095180095,0.146723824848781,
-4.99021296137976));
#41681=CARTESIAN_POINT('Ctrl Pts',(-72.2490202177595,-0.692631440740558,
-4.94395084387207));
#41682=CARTESIAN_POINT('Ctrl Pts',(-72.2885309175095,-1.47037247590722,
-4.70075073237942));
#41683=CARTESIAN_POINT('Ctrl Pts',(-72.3280416172596,-2.24811351107383,
-4.45755062088678));
#41684=CARTESIAN_POINT('Ctrl Pts',(-72.3675523170096,-2.96424031581777,
-4.01741251540921));
#41685=CARTESIAN_POINT('Ctrl Pts',(-72.4070630167596,-3.53214031702749,
-3.43290862203499));
#41686=CARTESIAN_POINT('Ctrl Pts',(-72.4465737165097,-4.10004031823723,
-2.84840472866075));
#41687=CARTESIAN_POINT('Ctrl Pts',(-72.4860844162597,-4.51971351591273,
-2.11953504738984));
#41688=CARTESIAN_POINT('Ctrl Pts',(-72.5255951160097,-4.74077108029855,
-1.3354637677462));
#41689=CARTESIAN_POINT('Ctrl Pts',(-72.5474495687053,-4.86304408772266,
-0.901772418331122));
#41690=CARTESIAN_POINT('Ctrl Pts',(-72.5693040214009,-4.92455064639084,
-0.451192141074852));
#41691=CARTESIAN_POINT('Ctrl Pts',(-72.5911584740964,-4.92473478262889,
-0.000479420352050008));
#41692=CARTESIAN_POINT('Ctrl Pts',(-72.8088415259036,-4.92403075528272,
-0.00394394407346908));
#41693=CARTESIAN_POINT('Ctrl Pts',(-72.7870416527649,-4.92794748682757,
-0.453990933627024));
#41694=CARTESIAN_POINT('Ctrl Pts',(-72.7652417796263,-4.87120978213869,
-0.903126684029842));
#41695=CARTESIAN_POINT('Ctrl Pts',(-72.7434419064877,-4.74985310581452,
-1.33422478502333));
#41696=CARTESIAN_POINT('Ctrl Pts',(-72.6644205069876,-4.30995263754923,
-2.89689329440753));
#41697=CARTESIAN_POINT('Ctrl Pts',(-72.5853991074877,-3.02098598707447,
-4.22255465662663));
#41698=CARTESIAN_POINT('Ctrl Pts',(-72.5063777079876,-1.47439201801798,
-4.7075043974958));
#41699=CARTESIAN_POINT('Ctrl Pts',(-72.4273563084875,0.0722019510385211,
-5.19245413836497));
#41700=CARTESIAN_POINT('Ctrl Pts',(-72.3483349089873,1.87642323867679,-4.83669225788416));
#41701=CARTESIAN_POINT('Ctrl Pts',(-72.2693135094873,3.13536286416929,-3.8053053582178));
#41702=CARTESIAN_POINT('Ctrl Pts',(-72.2298028097373,3.76483267691556,-3.28961190838461));
#41703=CARTESIAN_POINT('Ctrl Pts',(-72.1902921099873,4.25798207412539,-2.60501220375502));
#41704=CARTESIAN_POINT('Ctrl Pts',(-72.1507814102373,4.56314662709562,-1.84819336201149));
#41705=CARTESIAN_POINT('Ctrl Pts',(-72.1112707104872,4.86831118006585,-1.09137452026796));
#41706=CARTESIAN_POINT('Ctrl Pts',(-72.0717600107372,4.98549088879648,-0.262336541410498));
#41707=CARTESIAN_POINT('Ctrl Pts',(-72.0322493109872,4.89552659992533,0.546557739181261));
#41708=CARTESIAN_POINT('Ctrl Pts',(-71.9927386112371,4.80556231105419,1.35545201977297));
#41709=CARTESIAN_POINT('Ctrl Pts',(-71.9532279114871,4.50845402458131,2.14420260209896));
#41710=CARTESIAN_POINT('Ctrl Pts',(-71.9137172117371,4.04272711232429,2.81357323489973));
#41711=CARTESIAN_POINT('Ctrl Pts',(-71.8742065119871,3.57700020006725,3.48294386770051));
#41712=CARTESIAN_POINT('Ctrl Pts',(-71.834695812237,2.94265466202609,4.03293455097604));
#41713=CARTESIAN_POINT('Ctrl Pts',(-71.795185112487,2.21496146205706,4.39912726249893));
#41714=CARTESIAN_POINT('Ctrl Pts',(-71.755674412737,1.48726826208804,4.76531997402182));
#41715=CARTESIAN_POINT('Ctrl Pts',(-71.7161637129869,0.666227400191101,
4.94771471379208));
#41716=CARTESIAN_POINT('Ctrl Pts',(-71.6766530132369,-0.148363863695565,
4.92329807174835));
#41717=CARTESIAN_POINT('Ctrl Pts',(-71.6371423134869,-0.962955127582231,
4.89888142970463));
#41718=CARTESIAN_POINT('Ctrl Pts',(-71.5976316137369,-1.77109679345867,
4.66765340584695));
#41719=CARTESIAN_POINT('Ctrl Pts',(-71.5581209139868,-2.47553452990664,
4.25802563618345));
#41720=CARTESIAN_POINT('Ctrl Pts',(-71.5186102142368,-3.17997226635464,
3.84839786651993));
#41721=CARTESIAN_POINT('Ctrl Pts',(-71.4790995144868,-3.78070607337414,
3.26037035105059));
#41722=CARTESIAN_POINT('Ctrl Pts',(-71.4395888147368,-4.20503638745672,
2.56470212256411));
#41723=CARTESIAN_POINT('Ctrl Pts',(-71.4000781149867,-4.6293667015393,1.86903389407766));
#41724=CARTESIAN_POINT('Ctrl Pts',(-71.3605674152367,-4.87729352268495,
1.0657249525741));
#41725=CARTESIAN_POINT('Ctrl Pts',(-71.3210567154866,-4.91896083613891,
0.251894146567503));
#41726=CARTESIAN_POINT('Ctrl Pts',(-71.3169849856256,-4.92325481335249,
0.168025745967216));
#41727=CARTESIAN_POINT('Ctrl Pts',(-71.3129132557646,-4.92535829464761,
0.084045602148368));
#41728=CARTESIAN_POINT('Ctrl Pts',(-71.3088415259036,-4.92529298732208,
6.25886409129967E-5));
#41729=CARTESIAN_POINT('Origin',(-74.75,0.,0.));
#41730=CARTESIAN_POINT('',(-69.5911584740964,-4.92496870099469,-0.000124982963756182));
#41731=CARTESIAN_POINT('',(-69.8088415259036,-4.92497217740552,-0.000124998403726498));
#41732=CARTESIAN_POINT('',(-74.75,-4.925,-6.03138548580071E-16));
#41733=CARTESIAN_POINT('Ctrl Pts',(-69.5911584740964,-4.92496870099469,
-0.000124982963756182));
#41734=CARTESIAN_POINT('Ctrl Pts',(-69.6210472274001,-4.92435129484291,
0.616473474605334));
#41735=CARTESIAN_POINT('Ctrl Pts',(-69.6509359807039,-4.80819041294167,
1.23329802162961));
#41736=CARTESIAN_POINT('Ctrl Pts',(-69.6808247340076,-4.58206647380057,
1.80676283856513));
#41737=CARTESIAN_POINT('Ctrl Pts',(-69.7203354337577,-4.28314751338414,
2.56484049971359));
#41738=CARTESIAN_POINT('Ctrl Pts',(-69.7598461335077,-3.79206958950924,
3.24714761574599));
#41739=CARTESIAN_POINT('Ctrl Pts',(-69.7993568332577,-3.16812924736071,
3.77129715044878));
#41740=CARTESIAN_POINT('Ctrl Pts',(-69.8388675330078,-2.54418890521218,
4.29544668515157));
#41741=CARTESIAN_POINT('Ctrl Pts',(-69.8783782327578,-1.78738614479,4.66143863852477));
#41742=CARTESIAN_POINT('Ctrl Pts',(-69.9178889325078,-0.989103182537478,
4.82508031227747));
#41743=CARTESIAN_POINT('Ctrl Pts',(-69.9573996322578,-0.190820220284935,
4.98872198603017));
#41744=CARTESIAN_POINT('Ctrl Pts',(-69.9969103320079,0.648942943797969,
4.95001338016238));
#41745=CARTESIAN_POINT('Ctrl Pts',(-70.0364210317579,1.42878681291189,4.71362847149133));
#41746=CARTESIAN_POINT('Ctrl Pts',(-70.0759317315079,2.20863068202582,4.47724356282029));
#41747=CARTESIAN_POINT('Ctrl Pts',(-70.1154424312579,2.92855525617078,4.043182351346));
#41748=CARTESIAN_POINT('Ctrl Pts',(-70.154953131008,3.50163127605336,3.46385674265386));
#41749=CARTESIAN_POINT('Ctrl Pts',(-70.194463830758,4.0747072959359,2.88453113396175));
#41750=CARTESIAN_POINT('Ctrl Pts',(-70.233974530508,4.5009347615561,2.15994112805179));
#41751=CARTESIAN_POINT('Ctrl Pts',(-70.2734852302581,4.72884767388748,1.37757932621148));
#41752=CARTESIAN_POINT('Ctrl Pts',(-70.3129959300081,4.95676058621888,0.595217524371109));
#41753=CARTESIAN_POINT('Ctrl Pts',(-70.3525066297581,4.98635894526144,-0.244916073399569));
#41754=CARTESIAN_POINT('Ctrl Pts',(-70.3920173295082,4.81406881534808,-1.04137724504295));
#41755=CARTESIAN_POINT('Ctrl Pts',(-70.4315280292582,4.64177868543473,-1.83783841668626));
#41756=CARTESIAN_POINT('Ctrl Pts',(-70.4710387290082,4.26760006656548,-2.59062716220222));
#41757=CARTESIAN_POINT('Ctrl Pts',(-70.5105494287582,3.73671418001747,-3.20884594057165));
#41758=CARTESIAN_POINT('Ctrl Pts',(-70.5500601285083,3.20582829346942,-3.8270647189411));
#41759=CARTESIAN_POINT('Ctrl Pts',(-70.5895708282583,2.51823513924258,-4.31071353016401));
#41760=CARTESIAN_POINT('Ctrl Pts',(-70.6290815280083,1.75696002688706,-4.60139289329005));
#41761=CARTESIAN_POINT('Ctrl Pts',(-70.6685922277584,0.995684914531562,
-4.89207225641608));
#41762=CARTESIAN_POINT('Ctrl Pts',(-70.7081029275084,0.160727844047372,
-4.98978217144526));
#41763=CARTESIAN_POINT('Ctrl Pts',(-70.7476136272584,-0.647092004691638,
-4.88272435605896));
#41764=CARTESIAN_POINT('Ctrl Pts',(-70.7871243270084,-1.45491185343067,
-4.77566654067266));
#41765=CARTESIAN_POINT('Ctrl Pts',(-70.8266350267585,-2.23559448042453,
-4.46384099487087));
#41766=CARTESIAN_POINT('Ctrl Pts',(-70.8661457265085,-2.89487424539605,
-3.98490000982449));
#41767=CARTESIAN_POINT('Ctrl Pts',(-70.9056564262585,-3.55415401036755,
-3.50595902477813));
#41768=CARTESIAN_POINT('Ctrl Pts',(-70.9451671260085,-4.09203091331672,
-2.85990260048719));
#41769=CARTESIAN_POINT('Ctrl Pts',(-70.9846778257586,-4.44355750661547,
-2.12474045571216));
#41770=CARTESIAN_POINT('Ctrl Pts',(-71.0201713752045,-4.75934352406771,
-1.46432405961079));
#41771=CARTESIAN_POINT('Ctrl Pts',(-71.0556649246505,-4.92474626588707,
-0.732000028104022));
#41772=CARTESIAN_POINT('Ctrl Pts',(-71.0911584740964,-4.92530702679097,
7.89345770752653E-5));
#41773=CARTESIAN_POINT('Ctrl Pts',(-71.3088415259036,-4.92529298732208,
6.25886409129967E-5));
#41774=CARTESIAN_POINT('Ctrl Pts',(-71.2734025560146,-4.92472457428331,
-0.730897369035472));
#41775=CARTESIAN_POINT('Ctrl Pts',(-71.2379635861256,-4.75986224148064,
-1.46207471644967));
#41776=CARTESIAN_POINT('Ctrl Pts',(-71.2025246162366,-4.44501837891349,
-2.12168528048715));
#41777=CARTESIAN_POINT('Ctrl Pts',(-71.1630139164866,-4.09400080247182,
-2.85708123102559));
#41778=CARTESIAN_POINT('Ctrl Pts',(-71.1235032167365,-3.55655784382619,
-3.50352046159282));
#41779=CARTESIAN_POINT('Ctrl Pts',(-71.0839925169864,-2.89760438390271,
-3.98291704891334));
#41780=CARTESIAN_POINT('Ctrl Pts',(-71.0444818172364,-2.23865092397924,
-4.46231363623386));
#41781=CARTESIAN_POINT('Ctrl Pts',(-71.0049711174864,-1.4581869627779,-4.77466758030767));
#41782=CARTESIAN_POINT('Ctrl Pts',(-70.9654604177364,-0.650441891689018,
-4.8822776719318));
#41783=CARTESIAN_POINT('Ctrl Pts',(-70.9259497179864,0.157303179399837,
-4.98988776355592));
#41784=CARTESIAN_POINT('Ctrl Pts',(-70.8864390182364,0.99232936037624,-4.89275400273038));
#41785=CARTESIAN_POINT('Ctrl Pts',(-70.8469283184863,1.75380423846729,-4.60259771260765));
#41786=CARTESIAN_POINT('Ctrl Pts',(-70.8074176187363,2.51527911655836,-4.31244142248491));
#41787=CARTESIAN_POINT('Ctrl Pts',(-70.7679069189862,3.20320269176403,-3.82926260306501));
#41788=CARTESIAN_POINT('Ctrl Pts',(-70.7283962192362,3.73451218366536,-3.21140765367798));
#41789=CARTESIAN_POINT('Ctrl Pts',(-70.6888855194861,4.26582167556667,-2.59355270429097));
#41790=CARTESIAN_POINT('Ctrl Pts',(-70.6493748197361,4.64051708416361,-1.8410216249368));
#41791=CARTESIAN_POINT('Ctrl Pts',(-70.6098641199861,4.81335358220714,-1.04467902257766));
#41792=CARTESIAN_POINT('Ctrl Pts',(-70.5703534202361,4.98619008025067,-0.248336420218513));
#41793=CARTESIAN_POINT('Ctrl Pts',(-70.5308427204861,4.95716766774084,0.591817705145609));
#41794=CARTESIAN_POINT('Ctrl Pts',(-70.491332020736,4.72979133424381,1.37433574850428));
#41795=CARTESIAN_POINT('Ctrl Pts',(-70.451821320986,4.50241500074678,2.15685379186298));
#41796=CARTESIAN_POINT('Ctrl Pts',(-70.412310621236,4.07668474626254,2.88173575321616));
#41797=CARTESIAN_POINT('Ctrl Pts',(-70.372799921486,3.50400623574574,3.46145422727098));
#41798=CARTESIAN_POINT('Ctrl Pts',(-70.3332892217359,2.93132772522894,4.04117270132579));
#41799=CARTESIAN_POINT('Ctrl Pts',(-70.2937785219859,2.21170095867957,4.47572768808224));
#41800=CARTESIAN_POINT('Ctrl Pts',(-70.2542678222359,1.43201938322806,4.7126474368196));
#41801=CARTESIAN_POINT('Ctrl Pts',(-70.2147571224859,0.652337807776577,
4.94956718555696));
#41802=CARTESIAN_POINT('Ctrl Pts',(-70.1752464227358,-0.187398576577069,
4.98885169627524));
#41803=CARTESIAN_POINT('Ctrl Pts',(-70.1357357229858,-0.985793579818551,
4.82575756361085));
#41804=CARTESIAN_POINT('Ctrl Pts',(-70.0962250232358,-1.78418858306003,
4.66266343094646));
#41805=CARTESIAN_POINT('Ctrl Pts',(-70.0567143234858,-2.54124220518937,
4.29719065489939));
#41806=CARTESIAN_POINT('Ctrl Pts',(-70.0172036237357,-3.16554190244308,
3.7734691893382));
#41807=CARTESIAN_POINT('Ctrl Pts',(-69.9776929239857,-3.7898415996968,3.249747723777));
#41808=CARTESIAN_POINT('Ctrl Pts',(-69.9381822242356,-4.2813873720749,2.56777756870168));
#41809=CARTESIAN_POINT('Ctrl Pts',(-69.8986715244856,-4.58082620078788,
1.80990510032964));
#41810=CARTESIAN_POINT('Ctrl Pts',(-69.8687281916249,-4.80775704676852,
1.23554859108091));
#41811=CARTESIAN_POINT('Ctrl Pts',(-69.8387848587642,-4.92435274109235,
0.61759816956164));
#41812=CARTESIAN_POINT('Ctrl Pts',(-69.8088415259036,-4.92497217740552,
-0.000124998403726498));
#41813=CARTESIAN_POINT('Origin',(-74.75,0.,0.));
#41814=CARTESIAN_POINT('',(-68.0911584740964,-4.92463956541989,6.32542101904054E-5));
#41815=CARTESIAN_POINT('',(-68.3088415259036,-4.92463799521373,6.23586074887003E-5));
#41816=CARTESIAN_POINT('',(-74.75,-4.925,-6.03138548580071E-16));
#41817=CARTESIAN_POINT('Ctrl Pts',(-68.0911584740964,-4.92463956541989,
6.32542101904054E-5));
#41818=CARTESIAN_POINT('Ctrl Pts',(-68.1074081306498,-4.92479283391617,
0.335354424754706));
#41819=CARTESIAN_POINT('Ctrl Pts',(-68.1236577872031,-4.89104471897482,
0.670615165879185));
#41820=CARTESIAN_POINT('Ctrl Pts',(-68.1399074437565,-4.82308424351426,
0.998791021732417));
#41821=CARTESIAN_POINT('Ctrl Pts',(-68.1794181435065,-4.65783977007121,
1.79674374542491));
#41822=CARTESIAN_POINT('Ctrl Pts',(-68.2189288432566,-4.29032872667458,
2.55280998655433));
#41823=CARTESIAN_POINT('Ctrl Pts',(-68.2584395430066,-3.76492723805302,
3.1756964617695));
#41824=CARTESIAN_POINT('Ctrl Pts',(-68.2979502427567,-3.23952574943144,
3.7985829369847));
#41825=CARTESIAN_POINT('Ctrl Pts',(-68.3374609425067,-2.55623381558493,
4.28828964628564));
#41826=CARTESIAN_POINT('Ctrl Pts',(-68.3769716422567,-1.79755738736115,
4.58568561550747));
#41827=CARTESIAN_POINT('Ctrl Pts',(-68.4164823420067,-1.03888095913735,
4.88308158472931));
#41828=CARTESIAN_POINT('Ctrl Pts',(-68.4559930417568,-0.204820036536274,
4.98816681387202));
#41829=CARTESIAN_POINT('Ctrl Pts',(-68.4955037415068,0.603914416247443,
4.88825249992034));
#41830=CARTESIAN_POINT('Ctrl Pts',(-68.5350144412568,1.41264886903114,4.78833818596866));
#41831=CARTESIAN_POINT('Ctrl Pts',(-68.5745251410068,2.19605685199747,4.4834243289226));
#41832=CARTESIAN_POINT('Ctrl Pts',(-68.6140358407569,2.85954362849792,4.01032858527148));
#41833=CARTESIAN_POINT('Ctrl Pts',(-68.6535465405069,3.52303040499837,3.53723284162036));
#41834=CARTESIAN_POINT('Ctrl Pts',(-68.6930572402569,4.06659597503293,2.89595521136418));
#41835=CARTESIAN_POINT('Ctrl Pts',(-68.732567940007,4.42460602919109,2.16392851350848));
#41836=CARTESIAN_POINT('Ctrl Pts',(-68.772078639757,4.78261608334925,1.43190181565276));
#41837=CARTESIAN_POINT('Ctrl Pts',(-68.811589339507,4.955070621631,0.609126050197518));
#41838=CARTESIAN_POINT('Ctrl Pts',(-68.851100039257,4.92114614978146,-0.205050475785254));
#41839=CARTESIAN_POINT('Ctrl Pts',(-68.890610739007,4.88722167793191,-1.019227001768));
#41840=CARTESIAN_POINT('Ctrl Pts',(-68.9301214387571,4.64691819595108,-1.82480428827828));
#41841=CARTESIAN_POINT('Ctrl Pts',(-68.9696321385071,4.2292518041185,-2.52451070556032));
#41842=CARTESIAN_POINT('Ctrl Pts',(-69.0091428382571,3.81158541228592,-3.22421712284235));
#41843=CARTESIAN_POINT('Ctrl Pts',(-69.0486535380071,3.21655611060158,-3.81805267089615));
#41844=CARTESIAN_POINT('Ctrl Pts',(-69.0881642377572,2.51601233731885,-4.23431305450968));
#41845=CARTESIAN_POINT('Ctrl Pts',(-69.1276749375072,1.81546856403611,-4.65057343812322));
#41846=CARTESIAN_POINT('Ctrl Pts',(-69.1671856372573,1.00941031915496,-4.88925865729649));
#41847=CARTESIAN_POINT('Ctrl Pts',(-69.2066963370073,0.195167307063327,
-4.92154801331598));
#41848=CARTESIAN_POINT('Ctrl Pts',(-69.2462070367574,-0.619075705028329,
-4.95383736933547));
#41849=CARTESIAN_POINT('Ctrl Pts',(-69.2857177365074,-1.44150348433047,
-4.77973086220116));
#41850=CARTESIAN_POINT('Ctrl Pts',(-69.3252284362574,-2.17280974230828,
-4.4202514576521));
#41851=CARTESIAN_POINT('Ctrl Pts',(-69.3647391360074,-2.90411600028601,
-4.06077205310308));
#41852=CARTESIAN_POINT('Ctrl Pts',(-69.4042498357574,-3.54430073693943,
-3.51591975113934));
#41853=CARTESIAN_POINT('Ctrl Pts',(-69.4437605355075,-4.01606309768947,
-2.85148423114699));
#41854=CARTESIAN_POINT('Ctrl Pts',(-69.4832712352575,-4.48782545843955,
-2.18704871115457));
#41855=CARTESIAN_POINT('Ctrl Pts',(-69.5227819350075,-4.79116544328623,
-1.40302997313351));
#41856=CARTESIAN_POINT('Ctrl Pts',(-69.5622926347576,-4.88945543723059,
-0.594096500990709));
#41857=CARTESIAN_POINT('Ctrl Pts',(-69.5719145812038,-4.91339176495756,
-0.397098862457078));
#41858=CARTESIAN_POINT('Ctrl Pts',(-69.5815365276501,-4.92516745966715,
-0.198623638203757));
#41859=CARTESIAN_POINT('Ctrl Pts',(-69.5911584740964,-4.92496870099469,
-0.000124982963756182));
#41860=CARTESIAN_POINT('Ctrl Pts',(-69.8088415259036,-4.92497217740552,
-0.000124998403726498));
#41861=CARTESIAN_POINT('Ctrl Pts',(-69.7992741590142,-4.92517009707265,
-0.197497288638803));
#41862=CARTESIAN_POINT('Ctrl Pts',(-69.7897067921249,-4.91352796301374,
-0.394846378484991));
#41863=CARTESIAN_POINT('Ctrl Pts',(-69.7801394252355,-4.88986176534154,
-0.590742844833311));
#41864=CARTESIAN_POINT('Ctrl Pts',(-69.7406287254855,-4.7921266161344,-1.39974353995548));
#41865=CARTESIAN_POINT('Ctrl Pts',(-69.7011180257355,-4.48932443267227,
-2.18397014853107));
#41866=CARTESIAN_POINT('Ctrl Pts',(-69.6616073259854,-4.01801789610363,
-2.84872908003258));
#41867=CARTESIAN_POINT('Ctrl Pts',(-69.6220966262354,-3.54671135953497,
-3.51348801153412));
#41868=CARTESIAN_POINT('Ctrl Pts',(-69.5825859264854,-2.90690046985979,
-4.05877926596156));
#41869=CARTESIAN_POINT('Ctrl Pts',(-69.5430752267353,-2.17584093827506,
-4.41876016475229));
#41870=CARTESIAN_POINT('Ctrl Pts',(-69.5035645269853,-1.44478140669035,
-4.778741063543));
#41871=CARTESIAN_POINT('Ctrl Pts',(-69.4640538272353,-0.622473233196095,
-4.95341160669699));
#41872=CARTESIAN_POINT('Ctrl Pts',(-69.4245431274853,0.191791734706842,
-4.92168072074847));
#41873=CARTESIAN_POINT('Ctrl Pts',(-69.3850324277353,1.00605670260978,-4.88994983479994));
#41874=CARTESIAN_POINT('Ctrl Pts',(-69.3455217279852,1.8122784649214,-4.65181751974888));
#41875=CARTESIAN_POINT('Ctrl Pts',(-69.3060110282352,2.51310757343917,-4.23603771321305));
#41876=CARTESIAN_POINT('Ctrl Pts',(-69.2665003284852,3.21393668195695,-3.82025790667721));
#41877=CARTESIAN_POINT('Ctrl Pts',(-69.2269896287351,3.80937313668088,-3.22683060865659));
#41878=CARTESIAN_POINT('Ctrl Pts',(-69.1874789289851,4.2275193362816,-2.52741081868947));
#41879=CARTESIAN_POINT('Ctrl Pts',(-69.147968229235,4.64566553588232,-1.82799102872235));
#41880=CARTESIAN_POINT('Ctrl Pts',(-69.108457529485,4.88652148035984,-1.02257874680874));
#41881=CARTESIAN_POINT('Ctrl Pts',(-69.068946829735,4.92100436097563,-0.208425678976473));
#41882=CARTESIAN_POINT('Ctrl Pts',(-69.029436129985,4.95548724159141,0.60572738885575));
#41883=CARTESIAN_POINT('Ctrl Pts',(-68.989925430235,4.78359705834548,1.42862124260663));
#41884=CARTESIAN_POINT('Ctrl Pts',(-68.9504147304849,4.42608916083589,2.16089331641106));
#41885=CARTESIAN_POINT('Ctrl Pts',(-68.9109040307349,4.06858126332627,2.89316539021553));
#41886=CARTESIAN_POINT('Ctrl Pts',(-68.8713933309848,3.52545565155298,3.53481568407353));
#41887=CARTESIAN_POINT('Ctrl Pts',(-68.8318826312348,2.86229351099765,4.00836638064507));
#41888=CARTESIAN_POINT('Ctrl Pts',(-68.7923719314848,2.19913137044234,4.4819170772166));
#41889=CARTESIAN_POINT('Ctrl Pts',(-68.7528612317348,1.41593270110502,4.78736817650169));
#41890=CARTESIAN_POINT('Ctrl Pts',(-68.7133505319847,0.607266965471941,
4.88783715125428));
#41891=CARTESIAN_POINT('Ctrl Pts',(-68.6738398322347,-0.201398770161134,
4.98830612600687));
#41892=CARTESIAN_POINT('Ctrl Pts',(-68.6343291324847,-1.03553157208996,
4.88379297622697));
#41893=CARTESIAN_POINT('Ctrl Pts',(-68.5948184327347,-1.79441179684599,
4.58691742763232));
#41894=CARTESIAN_POINT('Ctrl Pts',(-68.5553077329847,-2.55329202160205,
4.29004187903766));
#41895=CARTESIAN_POINT('Ctrl Pts',(-68.5157970332346,-3.23691966918531,
3.80080393162825));
#41896=CARTESIAN_POINT('Ctrl Pts',(-68.4762863334846,-3.76274825208007,
3.17827795764013));
#41897=CARTESIAN_POINT('Ctrl Pts',(-68.4367756337345,-4.28857683497483,
2.55575198365201));
#41898=CARTESIAN_POINT('Ctrl Pts',(-68.3972649339845,-4.65660635318109,
1.79993798308518));
#41899=CARTESIAN_POINT('Ctrl Pts',(-68.3577542342345,-4.82239807731116,
1.0020987818121));
#41900=CARTESIAN_POINT('Ctrl Pts',(-68.3414499981242,-4.89081264431328,
0.672867490088553));
#41901=CARTESIAN_POINT('Ctrl Pts',(-68.3251457620139,-4.92478953903053,
0.336480018204721));
#41902=CARTESIAN_POINT('Ctrl Pts',(-68.3088415259036,-4.92463799521373,
6.23586074887003E-5));
#41903=CARTESIAN_POINT('Origin',(-74.75,0.,0.));
#41904=CARTESIAN_POINT('',(-66.5911584740964,-4.92536651616557,5.39754973401252E-5));
#41905=CARTESIAN_POINT('',(-66.8088415259036,-4.92536456956953,5.50140474394305E-5));
#41906=CARTESIAN_POINT('',(-74.75,-4.925,-6.03138548580071E-16));
#41907=CARTESIAN_POINT('Ctrl Pts',(-66.5911584740964,-4.92536651616557,
5.39754973401252E-5));
#41908=CARTESIAN_POINT('Ctrl Pts',(-66.5937690338994,-4.92539680548438,
0.0538966888551685));
#41909=CARTESIAN_POINT('Ctrl Pts',(-66.5963795937024,-4.92453210201228,
0.107738427698145));
#41910=CARTESIAN_POINT('Ctrl Pts',(-66.5989901535054,-4.92276614638168,
0.161550590117274));
#41911=CARTESIAN_POINT('Ctrl Pts',(-66.6385008532554,-4.89603849102888,
0.975995135615054));
#41912=CARTESIAN_POINT('Ctrl Pts',(-66.6780115530054,-4.66286388744967,
1.78366470433721));
#41913=CARTESIAN_POINT('Ctrl Pts',(-66.7175222527555,-4.25139764002992,
2.48703502819659));
#41914=CARTESIAN_POINT('Ctrl Pts',(-66.7570329525055,-3.83993139261016,
3.19040535205602));
#41915=CARTESIAN_POINT('Ctrl Pts',(-66.7965436522555,-3.25017350134988,
3.78947643105268));
#41916=CARTESIAN_POINT('Ctrl Pts',(-66.8360543520055,-2.5533358936523,4.21191179149275));
#41917=CARTESIAN_POINT('Ctrl Pts',(-66.8755650517556,-1.85649828595472,
4.63434715193282));
#41918=CARTESIAN_POINT('Ctrl Pts',(-66.9150757515056,-1.05258096181989,
4.88014679381625));
#41919=CARTESIAN_POINT('Ctrl Pts',(-66.9545864512556,-0.23865511431353,
4.91963096802401));
#41920=CARTESIAN_POINT('Ctrl Pts',(-66.9940971510057,0.57527073319281,4.95911514223177));
#41921=CARTESIAN_POINT('Ctrl Pts',(-67.0336078507557,1.39920510407067,4.79228384876389));
#41922=CARTESIAN_POINT('Ctrl Pts',(-67.0731185505057,2.13365979227223,4.43928158782135));
#41923=CARTESIAN_POINT('Ctrl Pts',(-67.1126292502557,2.86811448047378,4.08627932687882));
#41924=CARTESIAN_POINT('Ctrl Pts',(-67.1521399500058,3.51308948599901,3.54710609846165));
#41925=CARTESIAN_POINT('Ctrl Pts',(-67.1916506497558,3.99070554016657,2.88686584669476));
#41926=CARTESIAN_POINT('Ctrl Pts',(-67.2311613495058,4.46832159433413,2.22662559492788));
#41927=CARTESIAN_POINT('Ctrl Pts',(-67.2706720492559,4.77857869714402,1.44531831981123));
#41928=CARTESIAN_POINT('Ctrl Pts',(-67.3101827490059,4.88401400730307,0.637285102286454));
#41929=CARTESIAN_POINT('Ctrl Pts',(-67.3496934487559,4.98944931746212,-0.170748115238346));
#41930=CARTESIAN_POINT('Ctrl Pts',(-67.389204148506,4.89006283497034,-1.00550727517133));
#41931=CARTESIAN_POINT('Ctrl Pts',(-67.428714848256,4.59785525211343,-1.76619710274414));
#41932=CARTESIAN_POINT('Ctrl Pts',(-67.468225548006,4.30564766925652,-2.52688693031692));
#41933=CARTESIAN_POINT('Ctrl Pts',(-67.5077362477561,3.8206189860345,-3.21350742552951));
#41934=CARTESIAN_POINT('Ctrl Pts',(-67.5472469475061,3.20133531557612,-3.7431507213007));
#41935=CARTESIAN_POINT('Ctrl Pts',(-67.5867576472561,2.58205164511774,-4.2727940170719));
#41936=CARTESIAN_POINT('Ctrl Pts',(-67.6262683470061,1.828512987423,-4.64546011340169));
#41937=CARTESIAN_POINT('Ctrl Pts',(-67.6657790467562,1.03170742587757,-4.81615042461486));
#41938=CARTESIAN_POINT('Ctrl Pts',(-67.7052897465062,0.234901864332088,
-4.98684073582805));
#41939=CARTESIAN_POINT('Ctrl Pts',(-67.7448004462562,-0.605170601064078,
-4.95555526192458));
#41940=CARTESIAN_POINT('Ctrl Pts',(-67.7843111460062,-1.38707312596202,
-4.72607165290189));
#41941=CARTESIAN_POINT('Ctrl Pts',(-67.8238218457563,-2.16897565085989,
-4.49658804387921));
#41942=CARTESIAN_POINT('Ctrl Pts',(-67.8633325455063,-2.89270823525954,
-4.06890629973734));
#41943=CARTESIAN_POINT('Ctrl Pts',(-67.9028432452563,-3.47088181150553,
-3.49466802081241));
#41944=CARTESIAN_POINT('Ctrl Pts',(-67.9423539450063,-4.04905538775154,
-2.92042974188746));
#41945=CARTESIAN_POINT('Ctrl Pts',(-67.9818646447564,-4.48166995584387,
-2.19963492817945));
#41946=CARTESIAN_POINT('Ctrl Pts',(-68.0213753445064,-4.71648828814532,
-1.41931791819765));
#41947=CARTESIAN_POINT('Ctrl Pts',(-68.0446363877031,-4.85473234369457,
-0.959923683443132));
#41948=CARTESIAN_POINT('Ctrl Pts',(-68.0678974308997,-4.92442016477588,
-0.47989903766246));
#41949=CARTESIAN_POINT('Ctrl Pts',(-68.0911584740964,-4.92463956541989,
6.32542101904054E-5));
#41950=CARTESIAN_POINT('Ctrl Pts',(-68.3088415259036,-4.92463799521373,
6.23586074887003E-5));
#41951=CARTESIAN_POINT('Ctrl Pts',(-68.2856350622639,-4.92442229690989,
-0.47877419235977));
#41952=CARTESIAN_POINT('Ctrl Pts',(-68.2624285986241,-4.85506595209795,
-0.957671900476631));
#41953=CARTESIAN_POINT('Ctrl Pts',(-68.2392221349844,-4.71746064773569,
-1.41608270296097));
#41954=CARTESIAN_POINT('Ctrl Pts',(-68.1997114352344,-4.48317756397627,
-2.19656058448168));
#41955=CARTESIAN_POINT('Ctrl Pts',(-68.1602007354844,-4.05105746640354,
-2.91765194554378));
#41956=CARTESIAN_POINT('Ctrl Pts',(-68.1206900357343,-3.47327787646076,
-3.49228664021852));
#41957=CARTESIAN_POINT('Ctrl Pts',(-68.0811793359843,-2.89549828651797,
-4.06692133489327));
#41958=CARTESIAN_POINT('Ctrl Pts',(-68.0416686362342,-2.17205920420512,
-4.49509936318065));
#41959=CARTESIAN_POINT('Ctrl Pts',(-68.0021579364842,-1.3903142574668,-4.72511919955948));
#41960=CARTESIAN_POINT('Ctrl Pts',(-67.9626472367342,-0.608569310728499,
-4.95513903593829));
#41961=CARTESIAN_POINT('Ctrl Pts',(-67.9231365369842,0.231481500435274,
-4.98700068040857));
#41962=CARTESIAN_POINT('Ctrl Pts',(-67.8836258372341,1.02840394637516,-4.81685691168427));
#41963=CARTESIAN_POINT('Ctrl Pts',(-67.8441151374841,1.82532639231506,-4.64671314295996));
#41964=CARTESIAN_POINT('Ctrl Pts',(-67.8046044377341,2.57912047303106,-4.27456396104109));
#41965=CARTESIAN_POINT('Ctrl Pts',(-67.7650937379841,3.19876726338711,-3.74534553536036));
#41966=CARTESIAN_POINT('Ctrl Pts',(-67.725583038234,3.81841405374317,-3.21612710967962));
#41967=CARTESIAN_POINT('Ctrl Pts',(-67.686072338484,4.30391355373927,-2.52983944023701));
#41968=CARTESIAN_POINT('Ctrl Pts',(-67.646561638734,4.59664280018932,-1.76935020615716));
#41969=CARTESIAN_POINT('Ctrl Pts',(-67.6070509389839,4.88937204663936,-1.00886097207732));
#41970=CARTESIAN_POINT('Ctrl Pts',(-67.5675402392339,4.98933103954337,-0.174170173360232));
#41971=CARTESIAN_POINT('Ctrl Pts',(-67.5280295394839,4.8844499572822,0.63393516968748));
#41972=CARTESIAN_POINT('Ctrl Pts',(-67.4885188397338,4.77956887502102,1.44204051273519));
#41973=CARTESIAN_POINT('Ctrl Pts',(-67.4490081399838,4.46984771759466,2.22356040011353));
#41974=CARTESIAN_POINT('Ctrl Pts',(-67.4094974402338,3.99268461210709,2.88412807843272));
#41975=CARTESIAN_POINT('Ctrl Pts',(-67.3699867404838,3.5155215066195,3.54469575675192));
#41976=CARTESIAN_POINT('Ctrl Pts',(-67.3304760407338,2.87091645307069,4.08431122601196));
#41977=CARTESIAN_POINT('Ctrl Pts',(-67.2909653409837,2.13670404928016,4.43781714250942));
#41978=CARTESIAN_POINT('Ctrl Pts',(-67.2514546412337,1.40249164548963,4.79132305900688));
#41979=CARTESIAN_POINT('Ctrl Pts',(-67.2119439414836,0.578671891457383,
4.95871942274176));
#41980=CARTESIAN_POINT('Ctrl Pts',(-67.1724332417336,-0.235280846492803,
4.91979350256028));
#41981=CARTESIAN_POINT('Ctrl Pts',(-67.1329225419836,-1.04923358444297,
4.88086758237879));
#41982=CARTESIAN_POINT('Ctrl Pts',(-67.0934118422336,-1.85331930631107,
4.63561937828096));
#41983=CARTESIAN_POINT('Ctrl Pts',(-67.0539011424835,-2.55044648538715,
4.2136620545242));
#41984=CARTESIAN_POINT('Ctrl Pts',(-67.0143904427335,-3.24757366446323,
3.79170473076744));
#41985=CARTESIAN_POINT('Ctrl Pts',(-66.9748797429835,-3.83774230074728,
3.19303828735175));
#41986=CARTESIAN_POINT('Ctrl Pts',(-66.9353690432334,-4.24969087030623,
2.48995033914265));
#41987=CARTESIAN_POINT('Ctrl Pts',(-66.8958583434834,-4.66163943986517,
1.78686239093355));
#41988=CARTESIAN_POINT('Ctrl Pts',(-66.8563476437334,-4.895367942699,0.979352937931041));
#41989=CARTESIAN_POINT('Ctrl Pts',(-66.8168369439834,-4.92265419234351,
0.164926914612239));
#41990=CARTESIAN_POINT('Ctrl Pts',(-66.8141718046234,-4.92449474840484,
0.109990938681131));
#41991=CARTESIAN_POINT('Ctrl Pts',(-66.8115066652635,-4.92539599436154,
0.0550234924270285));
#41992=CARTESIAN_POINT('Ctrl Pts',(-66.8088415259036,-4.92536456956953,
5.50140474394305E-5));
#41993=CARTESIAN_POINT('Origin',(-74.75,0.,0.));
#41994=CARTESIAN_POINT('',(-65.0911584740964,-4.92488160240034,-0.000121459184743433));
#41995=CARTESIAN_POINT('',(-65.3088415259036,-4.92488488230248,-0.000121706157415094));
#41996=CARTESIAN_POINT('',(-74.75,-4.925,-6.03138548580071E-16));
#41997=CARTESIAN_POINT('Ctrl Pts',(-65.0911584740964,-4.92488160240034,
-0.000121459184743433));
#41998=CARTESIAN_POINT('Ctrl Pts',(-65.1196406368991,-4.9243274969235,0.587489219440107));
#41999=CARTESIAN_POINT('Ctrl Pts',(-65.1481227997017,-4.81907471229367,
1.17529310063035));
#42000=CARTESIAN_POINT('Ctrl Pts',(-65.1766049625043,-4.61328490383012,
1.72549341384484));
#42001=CARTESIAN_POINT('Ctrl Pts',(-65.2161156622544,-4.32781152211541,
2.48873599231131));
#42002=CARTESIAN_POINT('Ctrl Pts',(-65.2556263620044,-3.84886996389699,
3.17961623649651));
#42003=CARTESIAN_POINT('Ctrl Pts',(-65.2951370617544,-3.23429133576914,
3.71471192429474));
#42004=CARTESIAN_POINT('Ctrl Pts',(-65.3346477615044,-2.61971270764127,
4.24980761209299));
#42005=CARTESIAN_POINT('Ctrl Pts',(-65.3741584612545,-1.86949700960395,
4.62911874350427));
#42006=CARTESIAN_POINT('Ctrl Pts',(-65.4136691610045,-1.07423108520293,
4.80684435994266));
#42007=CARTESIAN_POINT('Ctrl Pts',(-65.4531798607546,-0.278965160801917,
4.98456997638105));
#42008=CARTESIAN_POINT('Ctrl Pts',(-65.4926905605046,0.561350989962814,
4.96071007784656));
#42009=CARTESIAN_POINT('Ctrl Pts',(-65.5322012602546,1.34525109828691,4.73814569295697));
#42010=CARTESIAN_POINT('Ctrl Pts',(-65.5717119600046,2.12915120661099,4.51558130806739));
#42011=CARTESIAN_POINT('Ctrl Pts',(-65.6112226597546,2.85663527249444,4.09431243682272));
#42012=CARTESIAN_POINT('Ctrl Pts',(-65.6507333595047,3.43986124540353,3.52520633970548));
#42013=CARTESIAN_POINT('Ctrl Pts',(-65.6902440592547,4.02308721831264,2.95610024258822));
#42014=CARTESIAN_POINT('Ctrl Pts',(-65.7297547590048,4.46205509824734,2.23915691959843));
#42015=CARTESIAN_POINT('Ctrl Pts',(-65.7692654587548,4.7037605095791,1.46094565047882));
#42016=CARTESIAN_POINT('Ctrl Pts',(-65.8087761585048,4.94546592091086,0.682734381359203));
#42017=CARTESIAN_POINT('Ctrl Pts',(-65.8482868582548,4.98990886363963,-0.156744833890189));
#42018=CARTESIAN_POINT('Ctrl Pts',(-65.8877975580048,4.83172295325732,-0.956126784529762));
#42019=CARTESIAN_POINT('Ctrl Pts',(-65.9273082577549,4.67353704287501,-1.75550873516929));
#42020=CARTESIAN_POINT('Ctrl Pts',(-65.9668189575049,4.31272227938163,-2.51479342119902));
#42021=CARTESIAN_POINT('Ctrl Pts',(-66.006329657255,3.79284622689918,-3.14229893934767));
#42022=CARTESIAN_POINT('Ctrl Pts',(-66.045840357005,3.27297017441671,-3.76980445749635));
#42023=CARTESIAN_POINT('Ctrl Pts',(-66.085351056755,2.59403283294513,-4.26553080776395));
#42024=CARTESIAN_POINT('Ctrl Pts',(-66.124861756505,1.83801434618199,-4.56962015799541));
#42025=CARTESIAN_POINT('Ctrl Pts',(-66.1643724562551,1.08199585941888,-4.87370950822687));
#42026=CARTESIAN_POINT('Ctrl Pts',(-66.2038831560051,0.248896227364141,
-4.98616185842222));
#42027=CARTESIAN_POINT('Ctrl Pts',(-66.2433938557551,-0.56068965944009,
-4.89339884241268));
#42028=CARTESIAN_POINT('Ctrl Pts',(-66.2829045555051,-1.37027554624432,
-4.80063582640315));
#42029=CARTESIAN_POINT('Ctrl Pts',(-66.3224152552551,-2.15634768779811,
-4.50265744418875));
#42030=CARTESIAN_POINT('Ctrl Pts',(-66.3619259550052,-2.82398965634758,
-4.03544390940708));
#42031=CARTESIAN_POINT('Ctrl Pts',(-66.4014366547552,-3.49163162489706,
-3.56823037462541));
#42032=CARTESIAN_POINT('Ctrl Pts',(-66.4409473545053,-4.04084342044216,
-2.93178168727652));
#42033=CARTESIAN_POINT('Ctrl Pts',(-66.4804580542553,-4.40530896465153,
-2.20294758246529));
#42034=CARTESIAN_POINT('Ctrl Pts',(-66.5173581942024,-4.74569345979552,
-1.5222691678622));
#42035=CARTESIAN_POINT('Ctrl Pts',(-66.5542583341494,-4.92493837806983,
-0.761010243661963));
#42036=CARTESIAN_POINT('Ctrl Pts',(-66.5911584740964,-4.92536651616557,
5.39754973401252E-5));
#42037=CARTESIAN_POINT('Ctrl Pts',(-66.8088415259036,-4.92536456956953,
5.50140474394305E-5));
#42038=CARTESIAN_POINT('Ctrl Pts',(-66.7719959655135,-4.92493012171699,
-0.759884379797087));
#42039=CARTESIAN_POINT('Ctrl Pts',(-66.7351504051234,-4.74623364618368,
-1.52002104452459));
#42040=CARTESIAN_POINT('Ctrl Pts',(-66.6983048447333,-4.40681886269117,
-2.19992561146736));
#42041=CARTESIAN_POINT('Ctrl Pts',(-66.6587941449832,-4.04285328693911,
-2.92900952059309));
#42042=CARTESIAN_POINT('Ctrl Pts',(-66.6192834452332,-3.4940781389798,-3.56583474520942));
#42043=CARTESIAN_POINT('Ctrl Pts',(-66.5797727454832,-2.82675677293931,
-4.03350608419058));
#42044=CARTESIAN_POINT('Ctrl Pts',(-66.5402620457332,-2.15943540689881,
-4.50117742317175));
#42045=CARTESIAN_POINT('Ctrl Pts',(-66.5007513459831,-1.37356782277715,
-4.79969487651773));
#42046=CARTESIAN_POINT('Ctrl Pts',(-66.4612406462331,-0.564045748482333,
-4.89301313897477));
#42047=CARTESIAN_POINT('Ctrl Pts',(-66.4217299464831,0.24547632581244,-4.9863314014318));
#42048=CARTESIAN_POINT('Ctrl Pts',(-66.382219246733,1.07865289028041,-4.8744504729999));
#42049=CARTESIAN_POINT('Ctrl Pts',(-66.342708546983,1.8348797649651,-4.57087972196626));
#42050=CARTESIAN_POINT('Ctrl Pts',(-66.303197847233,2.59110663964981,-4.26730897093261));
#42051=CARTESIAN_POINT('Ctrl Pts',(-66.2636871474829,3.2703838245513,-3.77204839729721));
#42052=CARTESIAN_POINT('Ctrl Pts',(-66.2241764477329,3.79069014064888,-3.14489959174344));
#42053=CARTESIAN_POINT('Ctrl Pts',(-66.1846657479829,4.31099645674646,-2.51775078618968));
#42054=CARTESIAN_POINT('Ctrl Pts',(-66.1451550482329,4.67233190404011,-1.75871374871756));
#42055=CARTESIAN_POINT('Ctrl Pts',(-66.1056443484829,4.83106604702023,-0.959440479596849));
#42056=CARTESIAN_POINT('Ctrl Pts',(-66.0661336487328,4.98980019000035,-0.160167210476135));
#42057=CARTESIAN_POINT('Ctrl Pts',(-66.0266229489828,4.94593302866694,0.679342290293157));
#42058=CARTESIAN_POINT('Ctrl Pts',(-65.9871122492328,4.70476142323086,1.45771915506364));
#42059=CARTESIAN_POINT('Ctrl Pts',(-65.9476015494827,4.46358981779478,2.23609601983415));
#42060=CARTESIAN_POINT('Ctrl Pts',(-65.9080908497327,4.02511376825602,2.95334024860583));
#42061=CARTESIAN_POINT('Ctrl Pts',(-65.8685801499827,3.44227826283868,3.52284622794538));
#42062=CARTESIAN_POINT('Ctrl Pts',(-65.8290694502326,2.85944275742136,4.09235220728492));
#42063=CARTESIAN_POINT('Ctrl Pts',(-65.7895587504826,2.13224779612549,4.51411993719233));
#42064=CARTESIAN_POINT('Ctrl Pts',(-65.7500480507326,1.34850052076172,4.73722192113332));
#42065=CARTESIAN_POINT('Ctrl Pts',(-65.7105373509825,0.564753245397947,
4.96032390507432));
#42066=CARTESIAN_POINT('Ctrl Pts',(-65.6710266512325,-0.275546344033775,
4.9847601430489));
#42067=CARTESIAN_POINT('Ctrl Pts',(-65.6315159514825,-1.0709339784724,4.8075800147594));
#42068=CARTESIAN_POINT('Ctrl Pts',(-65.5920052517325,-1.86632161291102,
4.6303998864699));
#42069=CARTESIAN_POINT('Ctrl Pts',(-65.5524945519824,-2.61679729235658,
4.25160339191634));
#42070=CARTESIAN_POINT('Ctrl Pts',(-65.5129838522324,-3.23174278109815,
3.71692934845159));
#42071=CARTESIAN_POINT('Ctrl Pts',(-65.4734731524824,-3.84668826983973,
3.18225530498682));
#42072=CARTESIAN_POINT('Ctrl Pts',(-65.4339624527323,-4.32610356787728,
2.49170371261087));
#42073=CARTESIAN_POINT('Ctrl Pts',(-65.3944517529823,-4.61210036560815,
1.72865710946905));
#42074=CARTESIAN_POINT('Ctrl Pts',(-65.3659150106227,-4.81866256228257,
1.17754400694317));
#42075=CARTESIAN_POINT('Ctrl Pts',(-65.3373782682632,-4.92432796707018,
0.588613870356569));
#42076=CARTESIAN_POINT('Ctrl Pts',(-65.3088415259036,-4.92488488230248,
-0.000121706157415094));
#42077=CARTESIAN_POINT('Origin',(-74.75,0.,0.));
#42078=CARTESIAN_POINT('',(-63.5911584740964,-4.92468790276689,8.47132295976605E-5));
#42079=CARTESIAN_POINT('',(-63.8088415259036,-4.92468576593835,8.39450088834838E-5));
#42080=CARTESIAN_POINT('',(-74.75,-4.925,-6.03138548580071E-16));
#42081=CARTESIAN_POINT('Ctrl Pts',(-63.5911584740964,-4.92468790276689,
8.47132295976605E-5));
#42082=CARTESIAN_POINT('Ctrl Pts',(-63.6060015401487,-4.92487782722442,
0.30634405253935));
#42083=CARTESIAN_POINT('Ctrl Pts',(-63.620844606201,-4.89675395020855,0.612568936338183));
#42084=CARTESIAN_POINT('Ctrl Pts',(-63.6356876722532,-4.8399842696057,0.913387866734746));
#42085=CARTESIAN_POINT('Ctrl Pts',(-63.6751983720033,-4.68886927777682,
1.71413660666273));
#42086=CARTESIAN_POINT('Ctrl Pts',(-63.7147090717532,-4.33477897649552,
2.47658043182792));
#42087=CARTESIAN_POINT('Ctrl Pts',(-63.7542197715033,-3.82046896632728,
3.10865598007547));
#42088=CARTESIAN_POINT('Ctrl Pts',(-63.7937304712533,-3.306158956159,3.74073152832308));
#42089=CARTESIAN_POINT('Ctrl Pts',(-63.8332411710034,-2.63162923710374,
4.24243879965303));
#42090=CARTESIAN_POINT('Ctrl Pts',(-63.8727518707534,-1.87832774245171,
4.55319777926076));
#42091=CARTESIAN_POINT('Ctrl Pts',(-63.9122625705035,-1.1250262477997,4.86395675886848));
#42092=CARTESIAN_POINT('Ctrl Pts',(-63.9517732702534,-0.292952977550855,
4.98376744675398));
#42093=CARTESIAN_POINT('Ctrl Pts',(-63.9912839700035,0.517421108612269,
4.89816297416606));
#42094=CARTESIAN_POINT('Ctrl Pts',(-64.0307946697535,1.32779519477542,4.81255850157814));
#42095=CARTESIAN_POINT('Ctrl Pts',(-64.0703053695035,2.11647009685286,4.52153886851682));
#42096=CARTESIAN_POINT('Ctrl Pts',(-64.1098160692536,2.78821510966239,4.06024403544654));
#42097=CARTESIAN_POINT('Ctrl Pts',(-64.1493267690036,3.45996012247191,3.59894920237627));
#42098=CARTESIAN_POINT('Ctrl Pts',(-64.1888374687536,4.01477524601345,2.96737916929708));
#42099=CARTESIAN_POINT('Ctrl Pts',(-64.2283481685037,4.38566781281213,2.24179458487893));
#42100=CARTESIAN_POINT('Ctrl Pts',(-64.2678588682537,4.75656037961082,1.51621000046075));
#42101=CARTESIAN_POINT('Ctrl Pts',(-64.3073695680038,4.94353038966664,0.696610864703609));
#42102=CARTESIAN_POINT('Ctrl Pts',(-64.3468802677538,4.92400163843868,-0.11803808615025));
#42103=CARTESIAN_POINT('Ctrl Pts',(-64.3863909675038,4.90447288721073,-0.932687037004086));
#42104=CARTESIAN_POINT('Ctrl Pts',(-64.4259016672538,4.67844537469903,-1.74238580295464));
#42105=CARTESIAN_POINT('Ctrl Pts',(-64.4654123670038,4.2732114102574,-2.44936509495314));
#42106=CARTESIAN_POINT('Ctrl Pts',(-64.5049230667538,3.86797744581578,-3.15634438695162));
#42107=CARTESIAN_POINT('Ctrl Pts',(-64.5444337665039,3.28353702944425,-3.76060420499805));
#42108=CARTESIAN_POINT('Ctrl Pts',(-64.5839444662539,2.59046001551689,-4.18918154692979));
#42109=CARTESIAN_POINT('Ctrl Pts',(-64.623455166004,1.89738300158948,-4.61775888886157));
#42110=CARTESIAN_POINT('Ctrl Pts',(-64.662965865754,1.09566939010621,-4.87065375467863));
#42111=CARTESIAN_POINT('Ctrl Pts',(-64.702476565504,0.282124280829646,-4.91732966306869));
#42112=CARTESIAN_POINT('Ctrl Pts',(-64.741987265254,-0.531420828446872,
-4.96400557145875));
#42113=CARTESIAN_POINT('Ctrl Pts',(-64.781497965004,-1.35679743551669,-4.80446252242183));
#42114=CARTESIAN_POINT('Ctrl Pts',(-64.8210086647541,-2.09434318758374,
-4.45796497717854));
#42115=CARTESIAN_POINT('Ctrl Pts',(-64.8605193645041,-2.83188893965079,
-4.11146743193524));
#42116=CARTESIAN_POINT('Ctrl Pts',(-64.9000300642541,-3.48160383671507,
-3.57801539048556));
#42117=CARTESIAN_POINT('Ctrl Pts',(-64.9395407640041,-3.96503627894513,
-2.9220219766076));
#42118=CARTESIAN_POINT('Ctrl Pts',(-64.9790514637542,-4.4484687211752,-2.26602856272963));
#42119=CARTESIAN_POINT('Ctrl Pts',(-65.0185621635042,-4.76561870857105,
-1.48749377642337));
#42120=CARTESIAN_POINT('Ctrl Pts',(-65.0580728632543,-4.87819109966346,
-0.680423926896355));
#42121=CARTESIAN_POINT('Ctrl Pts',(-65.0691014002016,-4.90961318993959,
-0.455148249397773));
#42122=CARTESIAN_POINT('Ctrl Pts',(-65.080129937149,-4.92509615677833,-0.227649337766092));
#42123=CARTESIAN_POINT('Ctrl Pts',(-65.0911584740964,-4.92488160240034,
-0.000121459184743433));
#42124=CARTESIAN_POINT('Ctrl Pts',(-65.3088415259036,-4.92488488230248,
-0.000121706157415094));
#42125=CARTESIAN_POINT('Ctrl Pts',(-65.2978675685131,-4.92509904704324,
-0.226523131011731));
#42126=CARTESIAN_POINT('Ctrl Pts',(-65.2868936111227,-4.90976947097626,
-0.452895783772063));
#42127=CARTESIAN_POINT('Ctrl Pts',(-65.2759196537322,-4.87865663849641,
-0.677077977943223));
#42128=CARTESIAN_POINT('Ctrl Pts',(-65.2364089539822,-4.76663781622961,
-1.48422484830604));
#42129=CARTESIAN_POINT('Ctrl Pts',(-65.1968982542322,-4.45002187427182,
-2.26297697512404));
#42130=CARTESIAN_POINT('Ctrl Pts',(-65.1573875544821,-3.96703946931719,
-2.91930180581596));
#42131=CARTESIAN_POINT('Ctrl Pts',(-65.1178768547321,-3.48405706436252,
-3.57562663650791));
#42132=CARTESIAN_POINT('Ctrl Pts',(-65.0783661549821,-2.83470819641105,
-4.10952417107375));
#42133=CARTESIAN_POINT('Ctrl Pts',(-65.0388554552321,-2.09740026810914,
-4.45652749345232));
#42134=CARTESIAN_POINT('Ctrl Pts',(-64.999344755482,-1.3600923398073,-4.80353081583086));
#42135=CARTESIAN_POINT('Ctrl Pts',(-64.959834055732,-0.534825351155019,
-4.96363992602214));
#42136=CARTESIAN_POINT('Ctrl Pts',(-64.920323355982,0.278751581226722,-4.91752201220536));
#42137=CARTESIAN_POINT('Ctrl Pts',(-64.8808126562319,1.09232851360851,-4.87140409838858));
#42138=CARTESIAN_POINT('Ctrl Pts',(-64.8413019564819,1.89421538971978,-4.61905916056376));
#42139=CARTESIAN_POINT('Ctrl Pts',(-64.8017912567319,2.58758618848735,-4.19095727748569));
#42140=CARTESIAN_POINT('Ctrl Pts',(-64.7622805569819,3.28095698725492,-3.76285539440761));
#42141=CARTESIAN_POINT('Ctrl Pts',(-64.7227698572319,3.86581170867873,-3.15899656607628));
#42142=CARTESIAN_POINT('Ctrl Pts',(-64.6832591574818,4.27153047198954,-2.45229537605597));
#42143=CARTESIAN_POINT('Ctrl Pts',(-64.6437484577318,4.67724923530035,-1.74559418603566));
#42144=CARTESIAN_POINT('Ctrl Pts',(-64.6042377579817,4.90383204049817,-0.936050634326364));
#42145=CARTESIAN_POINT('Ctrl Pts',(-64.5647270582317,4.9239195278971,-0.12141526820937));
#42146=CARTESIAN_POINT('Ctrl Pts',(-64.5252163584817,4.94400701529602,0.693220097907579));
#42147=CARTESIAN_POINT('Ctrl Pts',(-64.4857056587317,4.75759918489606,1.51294727843224));
#42148=CARTESIAN_POINT('Ctrl Pts',(-64.4461949589816,4.38720435932008,2.23878607600718));
#42149=CARTESIAN_POINT('Ctrl Pts',(-64.4066842592316,4.01680953374406,2.96462487358218));
#42150=CARTESIAN_POINT('Ctrl Pts',(-64.3671735594815,3.46242771299201,3.59657528820741));
#42151=CARTESIAN_POINT('Ctrl Pts',(-64.3276628597315,2.79099924420997,4.05833074100424));
#42152=CARTESIAN_POINT('Ctrl Pts',(-64.2881521599815,2.11957077542799,4.52008619380104));
#42153=CARTESIAN_POINT('Ctrl Pts',(-64.2486414602315,1.33109565861598,4.81164668476946));
#42154=CARTESIAN_POINT('Ctrl Pts',(-64.2091307604815,0.520780475338853,
4.8978069460797));
#42155=CARTESIAN_POINT('Ctrl Pts',(-64.1696200607315,-0.289534707938324,
4.98396720738995));
#42156=CARTESIAN_POINT('Ctrl Pts',(-64.1301093609814,-1.12168995768064,
4.86472723904205));
#42157=CARTESIAN_POINT('Ctrl Pts',(-64.0905986612314,-1.87520441536793,
4.55448499669779));
#42158=CARTESIAN_POINT('Ctrl Pts',(-64.0510879614814,-2.62871887305523,
4.24424275435354));
#42159=CARTESIAN_POINT('Ctrl Pts',(-64.0115772617313,-3.30359253868746,
3.74299823801292));
#42160=CARTESIAN_POINT('Ctrl Pts',(-63.9720665619813,-3.81833594820552,
3.11127558586541));
#42161=CARTESIAN_POINT('Ctrl Pts',(-63.9325558622312,-4.33307935772359,
2.47955293371789));
#42162=CARTESIAN_POINT('Ctrl Pts',(-63.8930451624812,-4.6876925111275,1.71735214576347));
#42163=CARTESIAN_POINT('Ctrl Pts',(-63.8535344627312,-4.83935667464416,
0.916707237965155));
#42164=CARTESIAN_POINT('Ctrl Pts',(-63.838636817122,-4.89654217057262,0.614821314135713));
#42165=CARTESIAN_POINT('Ctrl Pts',(-63.8237391715128,-4.92487454999785,
0.307469816571031));
#42166=CARTESIAN_POINT('Ctrl Pts',(-63.8088415259036,-4.92468576593835,
8.39450088834838E-5));
#42167=CARTESIAN_POINT('Origin',(-74.75,0.,0.));
#42168=CARTESIAN_POINT('',(-62.0911584740964,-4.92540487062078,2.56800769940328E-5));
#42169=CARTESIAN_POINT('',(-62.3088415259036,-4.92540385667628,2.68226834623546E-5));
#42170=CARTESIAN_POINT('',(-74.75,-4.925,-6.03138548580071E-16));
#42171=CARTESIAN_POINT('Ctrl Pts',(-62.0911584740964,-4.92540487062078,
2.56800769940328E-5));
#42172=CARTESIAN_POINT('Ctrl Pts',(-62.0923624433983,-4.92541209039183,
0.0248569463254631));
#42173=CARTESIAN_POINT('Ctrl Pts',(-62.0935664127002,-4.9252281978348,0.0496881052786896));
#42174=CARTESIAN_POINT('Ctrl Pts',(-62.0947703820021,-4.92485252944502,
0.074516362533359));
#42175=CARTESIAN_POINT('Ctrl Pts',(-62.1342810817521,-4.91252420767574,
0.889306088618798));
#42176=CARTESIAN_POINT('Ctrl Pts',(-62.1737917815022,-4.69366144066925,
1.70097080831941));
#42177=CARTESIAN_POINT('Ctrl Pts',(-62.2133024812522,-4.29469141098677,
2.41150384813135));
#42178=CARTESIAN_POINT('Ctrl Pts',(-62.2528131810022,-3.89572138130432,
3.12203688794325));
#42179=CARTESIAN_POINT('Ctrl Pts',(-62.2923238807522,-3.31664408894592,
3.73143824786648));
#42180=CARTESIAN_POINT('Ctrl Pts',(-62.3318345805023,-2.62738180324177,
4.16612409622118));
#42181=CARTESIAN_POINT('Ctrl Pts',(-62.3713452802523,-1.9381195175376,4.60080994457588));
#42182=CARTESIAN_POINT('Ctrl Pts',(-62.4108559800023,-1.13867223848768,
4.86078028136204));
#42183=CARTESIAN_POINT('Ctrl Pts',(-62.4503666797523,-0.325571411348048,
4.91464427819981));
#42184=CARTESIAN_POINT('Ctrl Pts',(-62.4898773795024,0.487529415791584,
4.96850827503758));
#42185=CARTESIAN_POINT('Ctrl Pts',(-62.5293880792524,1.31428379102092,4.81626593192696));
#42186=CARTESIAN_POINT('Ctrl Pts',(-62.5688987790024,2.05486299916099,4.47630016641082));
#42187=CARTESIAN_POINT('Ctrl Pts',(-62.6084094787525,2.7954422073011,4.13633440089467));
#42188=CARTESIAN_POINT('Ctrl Pts',(-62.6479201785025,3.44984624835192,3.60864521297299));
#42189=CARTESIAN_POINT('Ctrl Pts',(-62.6874308782526,3.93905731898545,2.95694987493439));
#42190=CARTESIAN_POINT('Ctrl Pts',(-62.7269415780026,4.42826838961897,2.3052545368958));
#42191=CARTESIAN_POINT('Ctrl Pts',(-62.7664522777526,4.75228648983517,1.52955304874031));
#42192=CARTESIAN_POINT('Ctrl Pts',(-62.8059629775026,4.87198716912245,0.723509605351551));
#42193=CARTESIAN_POINT('Ctrl Pts',(-62.8454736772526,4.99168784840973,-0.0825338380371624));
#42194=CARTESIAN_POINT('Ctrl Pts',(-62.8849843770027,4.9070711067681,-0.918919236659191));
#42195=CARTESIAN_POINT('Ctrl Pts',(-62.9244950767527,4.62835422378369,-1.68465495111375));
#42196=CARTESIAN_POINT('Ctrl Pts',(-62.9640057765027,4.34963734079928,-2.45039066556833));
#42197=CARTESIAN_POINT('Ctrl Pts',(-63.0035164762527,3.87682031647208,-3.14547669585548));
#42198=CARTESIAN_POINT('Ctrl Pts',(-63.0430271760028,3.26699473382334,-3.68598298073927));
#42199=CARTESIAN_POINT('Ctrl Pts',(-63.0825378757528,2.65716915117458,-4.22648926562307));
#42200=CARTESIAN_POINT('Ctrl Pts',(-63.1220485755028,1.91033501020428,-4.61241580510349));
#42201=CARTESIAN_POINT('Ctrl Pts',(-63.1615592752529,1.11667083911405,-4.79716284507845));
#42202=CARTESIAN_POINT('Ctrl Pts',(-63.2010699750029,0.323006668023829,
-4.9819098850534));
#42203=CARTESIAN_POINT('Ctrl Pts',(-63.2405806747529,-0.5174875331863,-4.96547742552289));
#42204=CARTESIAN_POINT('Ctrl Pts',(-63.280091374503,-1.30332399652472,-4.74984964869538));
#42205=CARTESIAN_POINT('Ctrl Pts',(-63.319602074253,-2.0891604598631,-4.53422187186789));
#42206=CARTESIAN_POINT('Ctrl Pts',(-63.359112774003,-2.82033918532976,-4.11939877774343));
#42207=CARTESIAN_POINT('Ctrl Pts',(-63.398623473753,-3.40857200062825,-3.55546931384058));
#42208=CARTESIAN_POINT('Ctrl Pts',(-63.4381341735031,-3.99680481592679,
-2.99153984993768));
#42209=CARTESIAN_POINT('Ctrl Pts',(-63.4776448732531,-4.44209172105713,
-2.27850401625637));
#42210=CARTESIAN_POINT('Ctrl Pts',(-63.5171555730031,-4.69066533243408,
-1.50245927207026));
#42211=CARTESIAN_POINT('Ctrl Pts',(-63.5418232067009,-4.8458567826278,-1.01795285725689));
#42212=CARTESIAN_POINT('Ctrl Pts',(-63.5664908403987,-4.92437226805018,
-0.508886490698715));
#42213=CARTESIAN_POINT('Ctrl Pts',(-63.5911584740964,-4.92468790276689,
8.47132295976605E-5));
#42214=CARTESIAN_POINT('Ctrl Pts',(-63.8088415259036,-4.92468576593835,
8.39450088834838E-5));
#42215=CARTESIAN_POINT('Ctrl Pts',(-63.7842284717628,-4.92437386750827,
-0.507761743991617));
#42216=CARTESIAN_POINT('Ctrl Pts',(-63.7596154176219,-4.84621118799329,
-1.01570125954844));
#42217=CARTESIAN_POINT('Ctrl Pts',(-63.7350023634811,-4.69169472196826,
-1.49924174849018));
#42218=CARTESIAN_POINT('Ctrl Pts',(-63.6954916637311,-4.4436534321463,-2.27545679950503));
#42219=CARTESIAN_POINT('Ctrl Pts',(-63.6559809639811,-3.99885567887296,
-2.98879787389256));
#42220=CARTESIAN_POINT('Ctrl Pts',(-63.616470264231,-3.41100978175644,-3.55313065525637));
#42221=CARTESIAN_POINT('Ctrl Pts',(-63.576959564481,-2.8231638846399,-4.1174634366202));
#42222=CARTESIAN_POINT('Ctrl Pts',(-63.537448864731,-2.09226984368017,-4.5327879249603));
#42223=CARTESIAN_POINT('Ctrl Pts',(-63.4979381649809,-1.30658145616534,
-4.74895463054403));
#42224=CARTESIAN_POINT('Ctrl Pts',(-63.4584274652309,-0.520893068650557,
-4.96512133612775));
#42225=CARTESIAN_POINT('Ctrl Pts',(-63.4189167654809,0.31958966541932,-4.98213025895514));
#42226=CARTESIAN_POINT('Ctrl Pts',(-63.3794060657308,1.11338036268379,-4.79792761018242));
#42227=CARTESIAN_POINT('Ctrl Pts',(-63.3398953659808,1.90717105994831,-4.6137249614097));
#42228=CARTESIAN_POINT('Ctrl Pts',(-63.3003846662308,2.65426972040742,-4.22831074103685));
#42229=CARTESIAN_POINT('Ctrl Pts',(-63.2608739664808,3.26446587573142,-3.68822284179601));
#42230=CARTESIAN_POINT('Ctrl Pts',(-63.2213632667307,3.87466203105542,-3.14813494255516));
#42231=CARTESIAN_POINT('Ctrl Pts',(-63.1818525669807,4.34795568124431,-2.45337336444632));
#42232=CARTESIAN_POINT('Ctrl Pts',(-63.1423418672306,4.62719769178514,-1.68782899184099));
#42233=CARTESIAN_POINT('Ctrl Pts',(-63.1028311674806,4.90643970232597,-0.922284619235678));
#42234=CARTESIAN_POINT('Ctrl Pts',(-63.0633204677306,4.99163007321876,-0.0859574521338825));
#42235=CARTESIAN_POINT('Ctrl Pts',(-63.0238097679806,4.87248226044709,0.720167901387682));
#42236=CARTESIAN_POINT('Ctrl Pts',(-62.9842990682306,4.75333444767542,1.52629325490925));
#42237=CARTESIAN_POINT('Ctrl Pts',(-62.9447883684805,4.4298484512393,2.30221679485058));
#42238=CARTESIAN_POINT('Ctrl Pts',(-62.9052776687305,3.94108447132522,2.95424751407866));
#42239=CARTESIAN_POINT('Ctrl Pts',(-62.8657669689805,3.45232049141112,3.60627823330677));
#42240=CARTESIAN_POINT('Ctrl Pts',(-62.8262562692304,2.79827852801906,4.13441613182161));
#42241=CARTESIAN_POINT('Ctrl Pts',(-62.7867455694804,2.05793266442289,4.47488975654842));
#42242=CARTESIAN_POINT('Ctrl Pts',(-62.7472348697304,1.31758680082672,4.81536338127524));
#42243=CARTESIAN_POINT('Ctrl Pts',(-62.7077241699804,0.490937037026456,
4.96817273221402));
#42244=CARTESIAN_POINT('Ctrl Pts',(-62.6682134702303,-0.322200543395056,
4.91486642691301));
#42245=CARTESIAN_POINT('Ctrl Pts',(-62.6287027704803,-1.13533812381655,
4.86156012161199));
#42246=CARTESIAN_POINT('Ctrl Pts',(-62.5891920707303,-1.93496352085928,
4.60213816007118));
#42247=CARTESIAN_POINT('Ctrl Pts',(-62.5496813709802,-2.62452378191686,
4.16792515560365));
#42248=CARTESIAN_POINT('Ctrl Pts',(-62.5101706712302,-3.31408404297441,
3.73371215113613));
#42249=CARTESIAN_POINT('Ctrl Pts',(-62.4706599714801,-3.89357916804681,
3.1247081037419));
#42250=CARTESIAN_POINT('Ctrl Pts',(-62.4311492717301,-4.2930364354653,2.41444887051428));
#42251=CARTESIAN_POINT('Ctrl Pts',(-62.3916385719801,-4.69249370288381,
1.70418963728662));
#42252=CARTESIAN_POINT('Ctrl Pts',(-62.3521278722301,-4.91191311264837,
0.89267521822563));
#42253=CARTESIAN_POINT('Ctrl Pts',(-62.3126171724801,-4.92480026881991,
0.0778941383738648));
#42254=CARTESIAN_POINT('Ctrl Pts',(-62.3113586236212,-4.92521076814783,
0.0519406168031391));
#42255=CARTESIAN_POINT('Ctrl Pts',(-62.3101000747624,-4.92541171219871,
0.0259837807572669));
#42256=CARTESIAN_POINT('Ctrl Pts',(-62.3088415259036,-4.92540385667628,
2.68226834623546E-5));
#42257=CARTESIAN_POINT('Origin',(-74.75,0.,0.));
#42258=CARTESIAN_POINT('',(-60.5911584740964,-4.92480136718117,-0.000112186803593595));
#42259=CARTESIAN_POINT('',(-60.8088415259036,-4.92480425490107,-0.00011264726956837));
#42260=CARTESIAN_POINT('',(-74.75,-4.925,-6.03138548580071E-16));
#42261=CARTESIAN_POINT('Ctrl Pts',(-60.5911584740964,-4.92480136718117,
-0.000112186803593595));
#42262=CARTESIAN_POINT('Ctrl Pts',(-60.618234046398,-4.92432726268177,0.558505514510406));
#42263=CARTESIAN_POINT('Ctrl Pts',(-60.6453096186995,-4.82941391746452,
1.11728024600357));
#42264=CARTESIAN_POINT('Ctrl Pts',(-60.672385191001,-4.64306200662679,1.64368490447722));
#42265=CARTESIAN_POINT('Ctrl Pts',(-60.7118958907511,-4.37112336337482,
2.41185394542412));
#42266=CARTESIAN_POINT('Ctrl Pts',(-60.7514065905011,-3.90446786036597,
3.11109147015909));
#42267=CARTESIAN_POINT('Ctrl Pts',(-60.7909172902511,-3.29944296942331,
3.6569661345086));
#42268=CARTESIAN_POINT('Ctrl Pts',(-60.8304279900011,-2.69441807848069,
4.20284079885807));
#42269=CARTESIAN_POINT('Ctrl Pts',(-60.8699386897512,-1.9510237996043,4.59535260282208));
#42270=CARTESIAN_POINT('Ctrl Pts',(-60.9094493895012,-1.15902336576893,
4.78710663625474));
#42271=CARTESIAN_POINT('Ctrl Pts',(-60.9489600892512,-0.36702293193357,
4.97886066968739));
#42272=CARTESIAN_POINT('Ctrl Pts',(-60.9884707890012,0.473583656860748,
4.96985693258868));
#42273=CARTESIAN_POINT('Ctrl Pts',(-61.0279814887513,1.26129509202582,4.76118260593435));
#42274=CARTESIAN_POINT('Ctrl Pts',(-61.0674921885013,2.04900652719094,4.55250827928001));
#42275=CARTESIAN_POINT('Ctrl Pts',(-61.1070028882514,2.7838228087268,4.14416336307003));
#42276=CARTESIAN_POINT('Ctrl Pts',(-61.1465135880014,3.37701652282332,3.58545457946338));
#42277=CARTESIAN_POINT('Ctrl Pts',(-61.1860242877514,3.97021023691983,3.02674579585673));
#42278=CARTESIAN_POINT('Ctrl Pts',(-61.2255349875014,4.421781383577,2.31767314485344));
#42279=CARTESIAN_POINT('Ctrl Pts',(-61.2650456872515,4.67720377868587,1.54385554044626));
#42280=CARTESIAN_POINT('Ctrl Pts',(-61.3045563870015,4.93262617379475,0.770037936039061));
#42281=CARTESIAN_POINT('Ctrl Pts',(-61.3440670867516,4.99189981735533,-0.0685246217720721));
#42282=CARTESIAN_POINT('Ctrl Pts',(-61.3835777865016,4.84786754771377,-0.870577606571574));
#42283=CARTESIAN_POINT('Ctrl Pts',(-61.4230884862516,4.70383527807222,-1.67263059137105));
#42284=CARTESIAN_POINT('Ctrl Pts',(-61.4625991860016,4.35649709522856,-2.43817400315895));
#42285=CARTESIAN_POINT('Ctrl Pts',(-61.5021098857517,3.84779329858565,-3.07477021171873));
#42286=CARTESIAN_POINT('Ctrl Pts',(-61.5416205855017,3.3390895019428,-3.71136642027844));
#42287=CARTESIAN_POINT('Ctrl Pts',(-61.5811312852517,2.66902009150075,-4.21901542561004));
#42288=CARTESIAN_POINT('Ctrl Pts',(-61.6206419850017,1.91849442749971,-4.53641976201257));
#42289=CARTESIAN_POINT('Ctrl Pts',(-61.6601526847518,1.16796876349859,-4.85382409841514));
#42290=CARTESIAN_POINT('Ctrl Pts',(-61.6996633845018,0.336986845938493,
-4.98098376588859));
#42291=CARTESIAN_POINT('Ctrl Pts',(-61.7391740842518,-0.474112143410631,
-4.90254452306669));
#42292=CARTESIAN_POINT('Ctrl Pts',(-61.7786847840019,-1.28521113275975,
-4.82410528024479));
#42293=CARTESIAN_POINT('Ctrl Pts',(-61.8181954837519,-2.07642719389789,
-4.54006712712753));
#42294=CARTESIAN_POINT('Ctrl Pts',(-61.8577061835019,-2.75222278267403,
-4.08472702631593));
#42295=CARTESIAN_POINT('Ctrl Pts',(-61.8972168832519,-3.42801837145014,
-3.62938692550436));
#42296=CARTESIAN_POINT('Ctrl Pts',(-61.936727583002,-3.98839348786427,-3.00274487699847));
#42297=CARTESIAN_POINT('Ctrl Pts',(-61.976238282752,-4.3656841078053,-2.28046648651042));
#42298=CARTESIAN_POINT('Ctrl Pts',(-62.0145450132002,-4.73147793505032,
-1.58019734959341));
#42299=CARTESIAN_POINT('Ctrl Pts',(-62.0528517436483,-4.92517515893018,
-0.790031526007394));
#42300=CARTESIAN_POINT('Ctrl Pts',(-62.0911584740964,-4.92540487062078,
2.56800769940328E-5));
#42301=CARTESIAN_POINT('Ctrl Pts',(-62.3088415259036,-4.92540385667628,
2.68226834623546E-5));
#42302=CARTESIAN_POINT('Ctrl Pts',(-62.2705893750124,-4.92516509707053,
-0.788905184172106));
#42303=CARTESIAN_POINT('Ctrl Pts',(-62.2323372241212,-4.73204013316386,
-1.57794991883566));
#42304=CARTESIAN_POINT('Ctrl Pts',(-62.19408507323,-4.36724718275288,-2.27747167475169));
#42305=CARTESIAN_POINT('Ctrl Pts',(-62.15457437348,-3.99045203793583,-3.00000866738299));
#42306=CARTESIAN_POINT('Ctrl Pts',(-62.1150636737299,-3.43050684572326,
-3.62703491200312));
#42307=CARTESIAN_POINT('Ctrl Pts',(-62.0755529739799,-2.75502371774203,
-4.08283841209044));
#42308=CARTESIAN_POINT('Ctrl Pts',(-62.0360422742299,-2.0795405897608,-4.53864191217776));
#42309=CARTESIAN_POINT('Ctrl Pts',(-61.9965315744799,-1.28851952601091,
-4.82322266773226));
#42310=CARTESIAN_POINT('Ctrl Pts',(-61.9570208747298,-0.477474525377241,
-4.9022181981402));
#42311=CARTESIAN_POINT('Ctrl Pts',(-61.9175101749798,0.3335704752564,-4.98121372854814));
#42312=CARTESIAN_POINT('Ctrl Pts',(-61.8779994752297,1.16463941277381,-4.85462403380952));
#42313=CARTESIAN_POINT('Ctrl Pts',(-61.8384887754797,1.91538259839802,-4.53773453237479));
#42314=CARTESIAN_POINT('Ctrl Pts',(-61.7989780757297,2.66612578402223,-4.22084503094005));
#42315=CARTESIAN_POINT('Ctrl Pts',(-61.7594673759797,3.33654321775324,-3.71365572280919));
#42316=CARTESIAN_POINT('Ctrl Pts',(-61.7199566762296,3.84568351541099,-3.07740856629143));
#42317=CARTESIAN_POINT('Ctrl Pts',(-61.6804459764796,4.35482381306875,-2.44116140977365));
#42318=CARTESIAN_POINT('Ctrl Pts',(-61.6409352767296,4.70268697465325,-1.67585640486897));
#42319=CARTESIAN_POINT('Ctrl Pts',(-61.6014245769795,4.84726931261692,-0.873902394698959));
#42320=CARTESIAN_POINT('Ctrl Pts',(-61.5619138772295,4.99185165058058,-0.0719483845289988));
#42321=CARTESIAN_POINT('Ctrl Pts',(-61.5224031774795,4.93315316492343,0.76665463090628));
#42322=CARTESIAN_POINT('Ctrl Pts',(-61.4828924777295,4.67826156456697,1.54064724001566));
#42323=CARTESIAN_POINT('Ctrl Pts',(-61.4433817779794,4.42336996421049,2.3146398491251));
#42324=CARTESIAN_POINT('Ctrl Pts',(-61.4038710782294,3.97228524915466,3.02402205190863));
#42325=CARTESIAN_POINT('Ctrl Pts',(-61.3643603784794,3.37947487548879,3.5831375567173));
#42326=CARTESIAN_POINT('Ctrl Pts',(-61.3248496787293,2.78666450182296,4.14225306152595));
#42327=CARTESIAN_POINT('Ctrl Pts',(-61.2853389789793,2.05212846954711,4.55110186835976));
#42328=CARTESIAN_POINT('Ctrl Pts',(-61.2458282792293,1.26456033791886,4.76031641137174));
#42329=CARTESIAN_POINT('Ctrl Pts',(-61.2063175794793,0.476992206290612,
4.96953095438371));
#42330=CARTESIAN_POINT('Ctrl Pts',(-61.1668068797292,-0.363608024690031,
4.97911123357385));
#42331=CARTESIAN_POINT('Ctrl Pts',(-61.1272961799792,-1.15573978373521,
4.78790045189409));
#42332=CARTESIAN_POINT('Ctrl Pts',(-61.0877854802292,-1.94787154278039,
4.59668967021432));
#42333=CARTESIAN_POINT('Ctrl Pts',(-61.0482747804792,-2.6915348298901,4.20468782766466));
#42334=CARTESIAN_POINT('Ctrl Pts',(-61.0087640807291,-3.29693399116305,
3.65922825755163));
#42335=CARTESIAN_POINT('Ctrl Pts',(-60.9692533809791,-3.90233315243601,
3.11376868743858));
#42336=CARTESIAN_POINT('Ctrl Pts',(-60.9297426812291,-4.36946818787219,
2.41485138976216));
#42337=CARTESIAN_POINT('Ctrl Pts',(-60.890231981479,-4.64193359992515,1.64686904231828));
#42338=CARTESIAN_POINT('Ctrl Pts',(-60.8631018296205,-4.82902287072889,
1.11953143902096));
#42339=CARTESIAN_POINT('Ctrl Pts',(-60.8359716777621,-4.9243268280576,0.559630166400692));
#42340=CARTESIAN_POINT('Ctrl Pts',(-60.8088415259036,-4.92480425490107,
-0.00011264726956837));
#42341=CARTESIAN_POINT('Origin',(-74.75,0.,0.));
#42342=CARTESIAN_POINT('',(-59.25,-4.925,-6.03138548580071E-16));
#42343=CARTESIAN_POINT('',(-59.3088415259036,-4.92475008045824,0.000102229393649578));
#42344=CARTESIAN_POINT('',(-74.75,-4.925,-6.03138548580071E-16));
#42345=CARTESIAN_POINT('',(-59.25,-3.87448963569914,3.04038732119116));
#42346=CARTESIAN_POINT('Origin',(-59.25,0.,0.));
#42347=CARTESIAN_POINT('Ctrl Pts',(-59.25,-3.87448963569905,3.04038732119127));
#42348=CARTESIAN_POINT('Ctrl Pts',(-59.2895106997501,-3.37129935567942,
3.68162322923889));
#42349=CARTESIAN_POINT('Ctrl Pts',(-59.3290213995001,-2.70610538505704,
4.19521969019135));
#42350=CARTESIAN_POINT('Ctrl Pts',(-59.3685320992501,-1.95853021177386,
4.51926688453211));
#42351=CARTESIAN_POINT('Ctrl Pts',(-59.4080427990001,-1.21095503849063,
4.84331407887289));
#42352=CARTESIAN_POINT('Ctrl Pts',(-59.4475534987502,-0.38099866254657,
4.97781200660196));
#42353=CARTESIAN_POINT('Ctrl Pts',(-59.4870641985002,0.430795782907827,
4.90654364883144));
#42354=CARTESIAN_POINT('Ctrl Pts',(-59.5265748982502,1.24259022836218,4.83527529106094));
#42355=CARTESIAN_POINT('Ctrl Pts',(-59.5660855980002,2.03622274332688,4.55824064779087));
#42356=CARTESIAN_POINT('Ctrl Pts',(-59.6055962977503,2.71600019639951,4.10889083869069));
#42357=CARTESIAN_POINT('Ctrl Pts',(-59.6451069975003,3.39577764947222,3.65954102959046));
#42358=CARTESIAN_POINT('Ctrl Pts',(-59.6846176972503,3.96170004065284,3.03787605466006));
#42359=CARTESIAN_POINT('Ctrl Pts',(-59.7241283970004,4.3453670671339,2.31896030760023));
#42360=CARTESIAN_POINT('Ctrl Pts',(-59.7636390967504,4.72903409361491,1.60004456054048));
#42361=CARTESIAN_POINT('Ctrl Pts',(-59.8031497965004,4.93044575539642,0.783878041351297));
#42362=CARTESIAN_POINT('Ctrl Pts',(-59.8426604962504,4.9253149473138,-0.0309888376303113));
#42363=CARTESIAN_POINT('Ctrl Pts',(-59.8821711960004,4.92018413923118,-0.845855716611944));
#42364=CARTESIAN_POINT('Ctrl Pts',(-59.9216818957505,4.70851086128444,-1.65942295538596));
#42365=CARTESIAN_POINT('Ctrl Pts',(-59.9611925955005,4.31583785436935,-2.37345423564581));
#42366=CARTESIAN_POINT('Ctrl Pts',(-60.0007032952506,3.92316484745423,-3.08748551590572));
#42367=CARTESIAN_POINT('Ctrl Pts',(-60.0402139950006,3.34949211157074,-3.7019808376514));
#42368=CARTESIAN_POINT('Ctrl Pts',(-60.0797246947506,2.66409743455116,-4.14274124495021));
#42369=CARTESIAN_POINT('Ctrl Pts',(-60.1192353945006,1.97870275753165,-4.58350165224898));
#42370=CARTESIAN_POINT('Ctrl Pts',(-60.1587460942507,1.18158613937606,-4.85052714510093));
#42371=CARTESIAN_POINT('Ctrl Pts',(-60.1982567940007,0.36899357827524,-4.91157502086969));
#42372=CARTESIAN_POINT('Ctrl Pts',(-60.2377674937508,-0.443598982825585,
-4.97262289663845));
#42373=CARTESIAN_POINT('Ctrl Pts',(-60.2772781935008,-1.27166748687167,
-4.82769315532402));
#42374=CARTESIAN_POINT('Ctrl Pts',(-60.3167888932508,-2.01522254205752,
-4.49428572454397));
#42375=CARTESIAN_POINT('Ctrl Pts',(-60.3562995930008,-2.75877759724342,
-4.16087829376391));
#42376=CARTESIAN_POINT('Ctrl Pts',(-60.3958102927509,-3.41781920356909,
-3.63899317351821));
#42377=CARTESIAN_POINT('Ctrl Pts',(-60.4353209925009,-3.91277057456095,
-2.99164681298116));
#42378=CARTESIAN_POINT('Ctrl Pts',(-60.4748316922509,-4.40772194555281,
-2.34430045244411));
#42379=CARTESIAN_POINT('Ctrl Pts',(-60.5143423920009,-4.73858308121087,
-1.57149285161571));
#42380=CARTESIAN_POINT('Ctrl Pts',(-60.553853091751,-4.86540275729235,-0.766538772622105));
#42381=CARTESIAN_POINT('Ctrl Pts',(-60.5662882191994,-4.90531647294471,
-0.51319710502857));
#42382=CARTESIAN_POINT('Ctrl Pts',(-60.5787233466479,-4.92501911141971,
-0.256671207364706));
#42383=CARTESIAN_POINT('Ctrl Pts',(-60.5911584740964,-4.92480136718117,
-0.000112186803593595));
#42384=CARTESIAN_POINT('Ctrl Pts',(-60.8088415259036,-4.92480425490107,
-0.00011264726956837));
#42385=CARTESIAN_POINT('Ctrl Pts',(-60.7964609780121,-4.92502212341619,
-0.255545154531168));
#42386=CARTESIAN_POINT('Ctrl Pts',(-60.7840804301205,-4.90549280940482,
-0.510944663455777));
#42387=CARTESIAN_POINT('Ctrl Pts',(-60.771699882229,-4.86592730455705,-0.763201574512367));
#42388=CARTESIAN_POINT('Ctrl Pts',(-60.7321891824789,-4.73965980846626,
-1.5682424466878));
#42389=CARTESIAN_POINT('Ctrl Pts',(-60.6926784827289,-4.40932902761496,
-2.34127679382733));
#42390=CARTESIAN_POINT('Ctrl Pts',(-60.6531677829788,-3.9148216471047,-2.98896247343204));
#42391=CARTESIAN_POINT('Ctrl Pts',(-60.6136570832288,-3.42031426659448,
-3.63664815303671));
#42392=CARTESIAN_POINT('Ctrl Pts',(-60.5741463834788,-2.76163028642532,
-4.15898516510658));
#42393=CARTESIAN_POINT('Ctrl Pts',(-60.5346356837288,-2.01830431751824,
-4.49290249811251));
#42394=CARTESIAN_POINT('Ctrl Pts',(-60.4951249839787,-1.27497834861111,
-4.82681983111845));
#42395=CARTESIAN_POINT('Ctrl Pts',(-60.4556142842287,-0.447010390966045,
-4.97231748506042));
#42396=CARTESIAN_POINT('Ctrl Pts',(-60.4161035844787,0.365624332431433,
-4.91182695300899));
#42397=CARTESIAN_POINT('Ctrl Pts',(-60.3765928847287,1.17825905582891,-4.85133642095756));
#42398=CARTESIAN_POINT('Ctrl Pts',(-60.3370821849786,1.9755605449788,-4.58485770291274));
#42399=CARTESIAN_POINT('Ctrl Pts',(-60.2975714852286,2.6612563944335,-4.14456749006351));
#42400=CARTESIAN_POINT('Ctrl Pts',(-60.2580607854786,3.34695224388815,-3.7042772772143));
#42401=CARTESIAN_POINT('Ctrl Pts',(-60.2185500857286,3.92104245364762,-3.09017556956071));
#42402=CARTESIAN_POINT('Ctrl Pts',(-60.1790393859785,4.31420705304533,-2.37641377416709));
#42403=CARTESIAN_POINT('Ctrl Pts',(-60.1395286862285,4.70737165244309,-1.66265197877339));
#42404=CARTESIAN_POINT('Ctrl Pts',(-60.1000179864784,4.91961064147904,-0.849230095639638));
#42405=CARTESIAN_POINT('Ctrl Pts',(-60.0605072867284,4.92529640254283,-0.0343669333774221));
#42406=CARTESIAN_POINT('Ctrl Pts',(-60.0209965869784,4.93098216360662,0.780496228884701));
#42407=CARTESIAN_POINT('Ctrl Pts',(-59.9814858872283,4.7301146966983,1.59680067027529));
#42408=CARTESIAN_POINT('Ctrl Pts',(-59.9419751874783,4.34694877854636,2.31597940409487));
#42409=CARTESIAN_POINT('Ctrl Pts',(-59.9024644877283,3.96378286039443,3.03515813791445));
#42410=CARTESIAN_POINT('Ctrl Pts',(-59.8629537879783,3.39831849099889,3.65721116416303));
#42411=CARTESIAN_POINT('Ctrl Pts',(-59.8234430882283,2.71883323159572,4.10702714690975));
#42412=CARTESIAN_POINT('Ctrl Pts',(-59.7839323884782,2.03934797219251,4.55684312965649));
#42413=CARTESIAN_POINT('Ctrl Pts',(-59.7444216887282,1.24584182278165,4.83442206890134));
#42414=CARTESIAN_POINT('Ctrl Pts',(-59.7049109889781,0.43413082165801,4.90624662373847));
#42415=CARTESIAN_POINT('Ctrl Pts',(-59.6654002892281,-0.37758017946563,
4.97807117857561));
#42416=CARTESIAN_POINT('Ctrl Pts',(-59.6258895894781,-1.20749603230206,
4.84414134900504));
#42417=CARTESIAN_POINT('Ctrl Pts',(-59.5863788897281,-1.95541025039442,
4.52062949002602));
#42418=CARTESIAN_POINT('Ctrl Pts',(-59.5468681899781,-2.70332446848675,
4.19711763104702));
#42419=CARTESIAN_POINT('Ctrl Pts',(-59.507357490228,-3.36923705183502,3.6840237426596));
#42420=CARTESIAN_POINT('Ctrl Pts',(-59.467846790478,-3.87273257024307,3.0433014749766));
#42421=CARTESIAN_POINT('Ctrl Pts',(-59.428336090728,-4.37622808865111,2.40257920729359));
#42422=CARTESIAN_POINT('Ctrl Pts',(-59.3888253909779,-4.71730654211892,
1.634228560315));
#42423=CARTESIAN_POINT('Ctrl Pts',(-59.3493146912279,-4.85479958887199,
0.831028695869623));
#42424=CARTESIAN_POINT('Ctrl Pts',(-59.3358236361198,-4.90174703051343,
0.556773526950549));
#42425=CARTESIAN_POINT('Ctrl Pts',(-59.3223325810117,-4.92495839013675,
0.278455277590655));
#42426=CARTESIAN_POINT('Ctrl Pts',(-59.3088415259036,-4.92475008045824,
0.000102229393649578));
#42427=CARTESIAN_POINT('Origin',(-92.3478126690739,0.,0.));
#42428=CARTESIAN_POINT('',(-60.0978126690739,-4.07033583047938,-9.27221085090139E-5));
#42429=CARTESIAN_POINT('',(-59.8021873309261,-4.07029344213305,8.44923339615722E-5));
#42430=CARTESIAN_POINT('',(-92.3478126690739,-4.0705,-4.39132641279065E-13));
#42431=CARTESIAN_POINT('',(-59.25,3.73370339826928,1.62162243917742));
#42432=CARTESIAN_POINT('Ctrl Pts',(-60.0978126690739,-4.07033583047938,
-9.27221085087783E-5));
#42433=CARTESIAN_POINT('Ctrl Pts',(-60.0853775416254,-4.07051579553988,
-0.212138101437242));
#42434=CARTESIAN_POINT('Ctrl Pts',(-60.0334317144269,-4.00249114200519,
-1.09781061344082));
#42435=CARTESIAN_POINT('Ctrl Pts',(-59.9419751874784,-3.36951511201551,
-2.57628189458803));
#42436=CARTESIAN_POINT('Ctrl Pts',(-59.8234430882282,-1.73542646721431,
-3.87029207649262));
#42437=CARTESIAN_POINT('Ctrl Pts',(-59.7049109889782,0.317763083477844,
-4.22964426655577));
#42438=CARTESIAN_POINT('Ctrl Pts',(-59.586378889728,2.29420766877876,-3.56755659021834));
#42439=CARTESIAN_POINT('Ctrl Pts',(-59.4678467904781,3.71662484933523,-2.04392011884845));
#42440=CARTESIAN_POINT('Ctrl Pts',(-59.3557204939019,4.21310320094652,-0.135703240697654));
#42441=CARTESIAN_POINT('Ctrl Pts',(-59.283104897076,3.95802532033354,1.10373061144362));
#42442=CARTESIAN_POINT('Ctrl Pts',(-59.25,3.73370339826928,1.62162243917742));
#42443=CARTESIAN_POINT('',(-59.25,2.75129702511905,-2.99988915288066));
#42444=CARTESIAN_POINT('Origin',(-59.25,0.,0.));
#42445=CARTESIAN_POINT('Ctrl Pts',(-59.8021873309261,-4.07029344213305,
8.44923339619191E-5));
#42446=CARTESIAN_POINT('Ctrl Pts',(-59.7761676862842,-4.0699613898905,-0.443619105718286));
#42447=CARTESIAN_POINT('Ctrl Pts',(-59.7106373418922,-3.88779319744078,
-1.56135382729816));
#42448=CARTESIAN_POINT('Ctrl Pts',(-59.6055962977503,-2.88282865866802,
-3.11125693021052));
#42449=CARTESIAN_POINT('Ctrl Pts',(-59.4870641985001,-1.05281798849905,
-4.10883397176923));
#42450=CARTESIAN_POINT('Ctrl Pts',(-59.3685320992501,1.03189169588001,-4.11422147186713));
#42451=CARTESIAN_POINT('Ctrl Pts',(-59.28951069975,2.25480927425104,-3.45523440144076));
#42452=CARTESIAN_POINT('Ctrl Pts',(-59.25,2.75129702511905,-2.99988915288066));
#42453=CARTESIAN_POINT('Origin',(-92.3478126690739,0.,0.));
#42454=CARTESIAN_POINT('',(-61.5978126690739,-4.07083462454048,2.1224518266207E-5));
#42455=CARTESIAN_POINT('',(-61.3021873309261,-4.07033821717255,-9.31026831621495E-5));
#42456=CARTESIAN_POINT('',(-92.3478126690739,-4.0705,-4.39132641279065E-13));
#42457=CARTESIAN_POINT('Ctrl Pts',(-61.5978126690739,-4.07083462454048,
2.12245182661715E-5));
#42458=CARTESIAN_POINT('Ctrl Pts',(-61.5595059386257,-4.0706447684112,-0.652959051089105));
#42459=CARTESIAN_POINT('Ctrl Pts',(-61.4816885084275,-3.74543265053492,
-1.97962494652396));
#42460=CARTESIAN_POINT('Ctrl Pts',(-61.3643603784794,-2.3700998720048,-3.51759714491556));
#42461=CARTESIAN_POINT('Ctrl Pts',(-61.2458282792293,-0.408285672900589,
-4.22186758284269));
#42462=CARTESIAN_POINT('Ctrl Pts',(-61.1272961799792,1.65212766441617,-3.90657615556305));
#42463=CARTESIAN_POINT('Ctrl Pts',(-61.0087640807291,3.31355966555602,-2.64786431219091));
#42464=CARTESIAN_POINT('Ctrl Pts',(-60.8902319814791,4.1747820452098,-0.749705251673546));
#42465=CARTESIAN_POINT('Ctrl Pts',(-60.7716998822289,4.02781349732346,1.32950422542484));
#42466=CARTESIAN_POINT('Ctrl Pts',(-60.6531677829789,2.90814627754596,3.08764446455717));
#42467=CARTESIAN_POINT('Ctrl Pts',(-60.5346356837287,1.08617490252564,4.10013257507453));
#42468=CARTESIAN_POINT('Ctrl Pts',(-60.4161035844787,-0.998102733832139,
4.12245727265436));
#42469=CARTESIAN_POINT('Ctrl Pts',(-60.2975714852285,-2.84134318794365,
3.14922724339409));
#42470=CARTESIAN_POINT('Ctrl Pts',(-60.191474513427,-3.87702460308865,1.59736017128054));
#42471=CARTESIAN_POINT('Ctrl Pts',(-60.1248882413754,-4.06994398431395,
0.461603390216087));
#42472=CARTESIAN_POINT('Ctrl Pts',(-60.0978126690739,-4.07033583047938,
-9.27221085087783E-5));
#42473=CARTESIAN_POINT('Ctrl Pts',(-61.3021873309261,-4.07033821717255,
-9.31026831620455E-5));
#42474=CARTESIAN_POINT('Ctrl Pts',(-61.2898067830346,-4.07051828494729,
-0.211207421628787));
#42475=CARTESIAN_POINT('Ctrl Pts',(-61.237915535393,-4.0028659545813,-1.09594776340383));
#42476=CARTESIAN_POINT('Ctrl Pts',(-61.1465135880014,-3.3712816981627,-2.57397025366613));
#42477=CARTESIAN_POINT('Ctrl Pts',(-61.0279814887513,-1.73807978469344,
-3.86910089790803));
#42478=CARTESIAN_POINT('Ctrl Pts',(-60.9094493895012,0.314860461962913,
-4.22986122300694));
#42479=CARTESIAN_POINT('Ctrl Pts',(-60.7909172902512,2.29176343348649,-3.56912927064055));
#42480=CARTESIAN_POINT('Ctrl Pts',(-60.672385191001,3.71521573733988,-2.04646876241471));
#42481=CARTESIAN_POINT('Ctrl Pts',(-60.553853091751,4.24146069462157,-0.0295953967523683));
#42482=CARTESIAN_POINT('Ctrl Pts',(-60.4353209925008,3.74341133987005,1.99442525015962));
#42483=CARTESIAN_POINT('Ctrl Pts',(-60.3167888932508,2.34134674152,3.53680099229865));
#42484=CARTESIAN_POINT('Ctrl Pts',(-60.1982567940007,0.373854285980798,
4.22505585861098));
#42485=CARTESIAN_POINT('Ctrl Pts',(-60.0797246947506,-1.68391575197083,
3.89297786596098));
#42486=CARTESIAN_POINT('Ctrl Pts',(-59.9611925955005,-3.33504093198254,
2.62076547651056));
#42487=CARTESIAN_POINT('Ctrl Pts',(-59.8686801408924,-3.99509770559378,
1.13384936119896));
#42488=CARTESIAN_POINT('Ctrl Pts',(-59.8156783860342,-4.07046560955365,
0.230142580189046));
#42489=CARTESIAN_POINT('Ctrl Pts',(-59.8021873309261,-4.07029344213305,
8.44923339619191E-5));
#42490=CARTESIAN_POINT('Origin',(-92.3478126690739,0.,0.));
#42491=CARTESIAN_POINT('',(-63.0978126690739,-4.07024205242896,7.0015268888928E-5));
#42492=CARTESIAN_POINT('',(-62.8021873309261,-4.07083378651793,2.21688792080826E-5));
#42493=CARTESIAN_POINT('',(-92.3478126690739,-4.0705,-4.39132641279065E-13));
#42494=CARTESIAN_POINT('Ctrl Pts',(-63.0978126690739,-4.07024205242896,
7.00152688889316E-5));
#42495=CARTESIAN_POINT('Ctrl Pts',(-63.0731450353761,-4.06998118113666,
-0.420593392972697));
#42496=CARTESIAN_POINT('Ctrl Pts',(-63.0089667019283,-3.90114800565978,
-1.51524740589905));
#42497=CARTESIAN_POINT('Ctrl Pts',(-62.9052776687305,-2.93532053926837,
-3.06182240003477));
#42498=CARTESIAN_POINT('Ctrl Pts',(-62.7867455694804,-1.12236845682437,
-4.09037310336489));
#42499=CARTESIAN_POINT('Ctrl Pts',(-62.6682134702303,0.961630515374074,
-4.13111726165049));
#42500=CARTESIAN_POINT('Ctrl Pts',(-62.5496813709802,2.81340008135553,-3.17421534553572));
#42501=CARTESIAN_POINT('Ctrl Pts',(-62.4311492717302,3.98574629304517,-1.4507548259719));
#42502=CARTESIAN_POINT('Ctrl Pts',(-62.31261717248,4.19555285965564,0.623056401494609));
#42503=CARTESIAN_POINT('Ctrl Pts',(-62.19408507323,3.39215244731244,2.5464023350196));
#42504=CARTESIAN_POINT('Ctrl Pts',(-62.0755529739799,1.7695626102988,3.85480365853339));
#42505=CARTESIAN_POINT('Ctrl Pts',(-61.9570208747298,-0.280368567998288,
4.23228738907051));
#42506=CARTESIAN_POINT('Ctrl Pts',(-61.8384887754797,-2.26259200924054,
3.58769291847877));
#42507=CARTESIAN_POINT('Ctrl Pts',(-61.7199566762296,-3.69840974642527,
2.07668688666092));
#42508=CARTESIAN_POINT('Ctrl Pts',(-61.6397313074277,-4.06570085141387,
0.714567436849348));
#42509=CARTESIAN_POINT('Ctrl Pts',(-61.5990166383758,-4.07084059166293,
0.0205442030491459));
#42510=CARTESIAN_POINT('Ctrl Pts',(-61.5978126690739,-4.07083462454048,
2.12245182661715E-5));
#42511=CARTESIAN_POINT('Ctrl Pts',(-62.8021873309261,-4.07083378651793,
2.21688792079568E-5));
#42512=CARTESIAN_POINT('Ctrl Pts',(-62.7639351800349,-4.07063645230967,
-0.652028132421247));
#42513=CARTESIAN_POINT('Ctrl Pts',(-62.6861723293937,-3.74615023682731,
-1.97777149888163));
#42514=CARTESIAN_POINT('Ctrl Pts',(-62.5688987790024,-2.37251192093704,
-3.51597074883963));
#42515=CARTESIAN_POINT('Ctrl Pts',(-62.4503666797524,-0.411181216372217,
-4.22158656537844));
#42516=CARTESIAN_POINT('Ctrl Pts',(-62.3318345805023,1.64944788626615,-3.90770838115492));
#42517=CARTESIAN_POINT('Ctrl Pts',(-62.2133024812522,3.3117428085009,-2.65013635349193));
#42518=CARTESIAN_POINT('Ctrl Pts',(-62.0947703820021,4.17426686894535,-0.752568421026256));
#42519=CARTESIAN_POINT('Ctrl Pts',(-61.976238282752,4.02872442070117,1.32674137044345));
#42520=CARTESIAN_POINT('Ctrl Pts',(-61.8577061835019,2.91026330437545,3.08564914085777));
#42521=CARTESIAN_POINT('Ctrl Pts',(-61.7391740842519,1.08898680526139,4.09938664434021));
#42522=CARTESIAN_POINT('Ctrl Pts',(-61.6206419850017,-0.995275066945756,
4.12314087364582));
#42523=CARTESIAN_POINT('Ctrl Pts',(-61.5021098857517,-2.83918252492348,
3.15117528982951));
#42524=CARTESIAN_POINT('Ctrl Pts',(-61.3959583343931,-3.87646153412254,
1.5992209574618));
#42525=CARTESIAN_POINT('Ctrl Pts',(-61.3293174827846,-4.06994362509825,
0.4625329121485));
#42526=CARTESIAN_POINT('Ctrl Pts',(-61.3021873309261,-4.07033821717255,
-9.31026831620455E-5));
#42527=CARTESIAN_POINT('Origin',(-92.3478126690739,0.,0.));
#42528=CARTESIAN_POINT('',(-64.5978126690739,-4.07040214468438,-0.000100385708283945));
#42529=CARTESIAN_POINT('',(-64.3021873309261,-4.0702402863456,6.93803360128642E-5));
#42530=CARTESIAN_POINT('',(-92.3478126690739,-4.0705,-4.39132641279065E-13));
#42531=CARTESIAN_POINT('Ctrl Pts',(-64.5978126690739,-4.07040214468438,
-0.000100385708283902));
#42532=CARTESIAN_POINT('Ctrl Pts',(-64.5867841321265,-4.07057947333322,
-0.188151599873747));
#42533=CARTESIAN_POINT('Ctrl Pts',(-64.536244895429,-4.01193778252147,-1.04980305045492));
#42534=CARTESIAN_POINT('Ctrl Pts',(-64.4461949589816,-3.41452444788805,
-2.51632388066006));
#42535=CARTESIAN_POINT('Ctrl Pts',(-64.3276628597316,-1.80356130768488,
-3.83901415561695));
#42536=CARTESIAN_POINT('Ctrl Pts',(-64.2091307604814,0.242953704951307,
-4.23459993090915));
#42537=CARTESIAN_POINT('Ctrl Pts',(-64.0905986612314,2.23079650020559,-3.60754903671119));
#42538=CARTESIAN_POINT('Ctrl Pts',(-63.9720665619813,3.67991206254491,-2.10929141882807));
#42539=CARTESIAN_POINT('Ctrl Pts',(-63.8535344627312,4.24034555879598,-0.101649493872672));
#42540=CARTESIAN_POINT('Ctrl Pts',(-63.7350023634811,3.77675484249208,1.93054032263455));
#42541=CARTESIAN_POINT('Ctrl Pts',(-63.6164702642311,2.40109496815141,3.49651341074552));
#42542=CARTESIAN_POINT('Ctrl Pts',(-63.4979381649809,0.445581553589111,
4.21809437503554));
#42543=CARTESIAN_POINT('Ctrl Pts',(-63.3794060657309,-1.61753778440945,
3.92102468668754));
#42544=CARTESIAN_POINT('Ctrl Pts',(-63.2608739664807,-3.29002908679384,
2.67704532753104));
#42545=CARTESIAN_POINT('Ctrl Pts',(-63.1670095009284,-3.98528076530966,
1.17999684215322));
#42546=CARTESIAN_POINT('Ctrl Pts',(-63.1126557351261,-4.07039902451109,
0.253192581900508));
#42547=CARTESIAN_POINT('Ctrl Pts',(-63.0978126690739,-4.07024205242896,
7.00152688889316E-5));
#42548=CARTESIAN_POINT('Ctrl Pts',(-64.3021873309261,-4.0702402863456,6.93803360126907E-5));
#42549=CARTESIAN_POINT('Ctrl Pts',(-64.2775742767853,-4.06998250308468,
-0.419663792674221));
#42550=CARTESIAN_POINT('Ctrl Pts',(-64.2134505228944,-3.90167851966751,
-1.51338581363879));
#42551=CARTESIAN_POINT('Ctrl Pts',(-64.1098160692536,-2.93741985505644,
-3.05980844446182));
#42552=CARTESIAN_POINT('Ctrl Pts',(-63.9912839700035,-1.12517364567985,
-4.08960235093184));
#42553=CARTESIAN_POINT('Ctrl Pts',(-63.8727518707534,0.95879689383177,-4.13177584557272));
#42554=CARTESIAN_POINT('Ctrl Pts',(-63.7542197715033,2.81122233387158,-3.17614422078426));
#42555=CARTESIAN_POINT('Ctrl Pts',(-63.6356876722533,3.98475033575612,-1.45348817792618));
#42556=CARTESIAN_POINT('Ctrl Pts',(-63.5171555730031,4.1959792117271,0.620178664929396));
#42557=CARTESIAN_POINT('Ctrl Pts',(-63.3986234737531,3.39389814665504,2.54407517416668));
#42558=CARTESIAN_POINT('Ctrl Pts',(-63.2800913745029,1.77220607843935,3.85358907217963));
#42559=CARTESIAN_POINT('Ctrl Pts',(-63.1615592752529,-0.277465716615854,
4.23247869430933));
#42560=CARTESIAN_POINT('Ctrl Pts',(-63.0430271760028,-2.26013080006508,
3.58924391596298));
#42561=CARTESIAN_POINT('Ctrl Pts',(-62.9244950767527,-3.69698455028266,
2.07922301753555));
#42562=CARTESIAN_POINT('Ctrl Pts',(-62.8442151283938,-4.06546031589444,
0.716429282973149));
#42563=CARTESIAN_POINT('Ctrl Pts',(-62.803445879785,-4.07084027908729,0.0214755288467767));
#42564=CARTESIAN_POINT('Ctrl Pts',(-62.8021873309261,-4.07083378651793,
2.21688792079568E-5));
#42565=CARTESIAN_POINT('Origin',(-92.3478126690739,0.,0.));
#42566=CARTESIAN_POINT('',(-66.0978126690738,-4.0708029246806,4.46106111926773E-5));
#42567=CARTESIAN_POINT('',(-65.8021873309261,-4.07040485551518,-0.000100589830685782));
#42568=CARTESIAN_POINT('',(-92.3478126690739,-4.0705,-4.39132641279065E-13));
#42569=CARTESIAN_POINT('Ctrl Pts',(-66.0978126690738,-4.0708029246806,4.46106111927618E-5));
#42570=CARTESIAN_POINT('Ctrl Pts',(-66.0609125291268,-4.07044906963106,
-0.628973034888802));
#42571=CARTESIAN_POINT('Ctrl Pts',(-65.9845016894298,-3.76367733983292,
-1.93184242303918));
#42572=CARTESIAN_POINT('Ctrl Pts',(-65.8685801499826,-2.43190252088865,
-3.47515657294758));
#42573=CARTESIAN_POINT('Ctrl Pts',(-65.7500480507326,-0.482842631226866,
-4.21399170277722));
#42574=CARTESIAN_POINT('Ctrl Pts',(-65.6315159514825,1.58282156305449,-3.93516695670401));
#42575=CARTESIAN_POINT('Ctrl Pts',(-65.5129838522324,3.26624153165954,-2.70601724578163));
#42576=CARTESIAN_POINT('Ctrl Pts',(-65.3944517529823,4.16087899042085,-0.823376648126326));
#42577=CARTESIAN_POINT('Ctrl Pts',(-65.2759196537323,4.05068305232286,1.25810567411077));
#42578=CARTESIAN_POINT('Ctrl Pts',(-65.1573875544821,2.96226553641969,3.03576118450472));
#42579=CARTESIAN_POINT('Ctrl Pts',(-65.0388554552321,1.1584743342804,4.08029414312485));
#42580=CARTESIAN_POINT('Ctrl Pts',(-64.9203233559819,-0.925083163194395,
4.13945457986673));
#42581=CARTESIAN_POINT('Ctrl Pts',(-64.8017912567319,-2.78523727417561,
3.19895551768826));
#42582=CARTESIAN_POINT('Ctrl Pts',(-64.6942876944292,-3.8622781385591,1.64530822478956));
#42583=CARTESIAN_POINT('Ctrl Pts',(-64.6262948318765,-4.06994417791418,
0.485558348777591));
#42584=CARTESIAN_POINT('Ctrl Pts',(-64.5978126690739,-4.07040214468438,
-0.000100385708283902));
#42585=CARTESIAN_POINT('Ctrl Pts',(-65.8021873309261,-4.07040485551518,
-0.000100589830685713));
#42586=CARTESIAN_POINT('Ctrl Pts',(-65.7912133735357,-4.07058186212983,
-0.187220792849738));
#42587=CARTESIAN_POINT('Ctrl Pts',(-65.7407287163952,-4.01229538452908,
-1.04794026068607));
#42588=CARTESIAN_POINT('Ctrl Pts',(-65.6507333595047,-3.41624951217949,
-2.51398138263055));
#42589=CARTESIAN_POINT('Ctrl Pts',(-65.5322012602546,-1.80619393837446,
-3.83777625437688));
#42590=CARTESIAN_POINT('Ctrl Pts',(-65.4136691610045,0.240049276229987,
-4.23476557399121));
#42591=CARTESIAN_POINT('Ctrl Pts',(-65.2951370617545,2.22832167981034,-3.60907822206265));
#42592=CARTESIAN_POINT('Ctrl Pts',(-65.1766049625043,3.6784645083721,-2.11181485512497));
#42593=CARTESIAN_POINT('Ctrl Pts',(-65.0580728632543,4.24027484861026,-0.104557782698988));
#42594=CARTESIAN_POINT('Ctrl Pts',(-64.9395407640041,3.77807805248247,1.92794951983446));
#42595=CARTESIAN_POINT('Ctrl Pts',(-64.8210086647541,2.4034925491091,3.4948657610925));
#42596=CARTESIAN_POINT('Ctrl Pts',(-64.7024765655039,0.448474500591471,
4.21778777844487));
#42597=CARTESIAN_POINT('Ctrl Pts',(-64.583944466254,-1.61484810493722,3.92213318484474));
#42598=CARTESIAN_POINT('Ctrl Pts',(-64.4654123670038,-3.2881922202403,2.67930122316078));
#42599=CARTESIAN_POINT('Ctrl Pts',(-64.3714933218946,-3.98487537838422,
1.18185972389678));
#42600=CARTESIAN_POINT('Ctrl Pts',(-64.3170849765353,-4.07039631589167,
0.254123023015174));
#42601=CARTESIAN_POINT('Ctrl Pts',(-64.3021873309261,-4.0702402863456,6.93803360126907E-5));
#42602=CARTESIAN_POINT('Origin',(-92.3478126690739,0.,0.));
#42603=CARTESIAN_POINT('',(-67.5978126690739,-4.07020210173435,5.22794437556925E-5));
#42604=CARTESIAN_POINT('',(-67.3021873309261,-4.07080131582391,4.54689699823894E-5));
#42605=CARTESIAN_POINT('',(-92.3478126690739,-4.0705,-4.39132641279065E-13));
#42606=CARTESIAN_POINT('Ctrl Pts',(-67.5978126690739,-4.07020210173435,
5.22794437558469E-5));
#42607=CARTESIAN_POINT('Ctrl Pts',(-67.5745516258772,-4.07002076765889,
-0.396635336610467));
#42608=CARTESIAN_POINT('Ctrl Pts',(-67.5117798829305,-3.91459128202717,
-1.46726694234189));
#42609=CARTESIAN_POINT('Ctrl Pts',(-67.4094974402338,-2.98897915866447,
-3.00946285351303));
#42610=CARTESIAN_POINT('Ctrl Pts',(-67.2909653409837,-1.19448972629963,
-4.06989648165282));
#42611=CARTESIAN_POINT('Ctrl Pts',(-67.1724332417337,0.888463555159219,
-4.14746857598213));
#42612=CARTESIAN_POINT('Ctrl Pts',(-67.0539011424835,2.75685691930934,-3.22344582769147));
#42613=CARTESIAN_POINT('Ctrl Pts',(-66.9353690432335,3.95948184624652,-1.52097553788664));
#42614=CARTESIAN_POINT('Ctrl Pts',(-66.8168369439834,4.20590987283498,0.548803443132984));
#42615=CARTESIAN_POINT('Ctrl Pts',(-66.6983048447332,3.43662974878158,2.48604888274442));
#42616=CARTESIAN_POINT('Ctrl Pts',(-66.5797727454832,1.83741913355893,3.82292479722488));
#42617=CARTESIAN_POINT('Ctrl Pts',(-66.4612406462331,-0.205519865420819,
4.23658171908943));
#42618=CARTESIAN_POINT('Ctrl Pts',(-66.3427085469829,-2.19882674941518,
3.62712337861033));
#42619=CARTESIAN_POINT('Ctrl Pts',(-66.224176447733,-3.66112695025279,2.1417311996929));
#42620=CARTESIAN_POINT('Ctrl Pts',(-66.1425444884298,-4.059296707607,0.762551858271784));
#42621=CARTESIAN_POINT('Ctrl Pts',(-66.1004232288768,-4.07082795872572,
0.0445454765449013));
#42622=CARTESIAN_POINT('Ctrl Pts',(-66.0978126690738,-4.0708029246806,4.46106111927618E-5));
#42623=CARTESIAN_POINT('Ctrl Pts',(-67.3021873309261,-4.07080131582391,
4.54689699825889E-5));
#42624=CARTESIAN_POINT('Ctrl Pts',(-67.265341770536,-4.07044224577636,-0.628042511262155));
#42625=CARTESIAN_POINT('Ctrl Pts',(-67.1889855103959,-3.76437490242843,
-1.92998766076815));
#42626=CARTESIAN_POINT('Ctrl Pts',(-67.0731185505057,-2.43428544669007,
-3.47348779841137));
#42627=CARTESIAN_POINT('Ctrl Pts',(-66.9545864512557,-0.485732755623718,
-4.21365955100716));
#42628=CARTESIAN_POINT('Ctrl Pts',(-66.8360543520056,1.58012219199054,-3.93625164084547));
#42629=CARTESIAN_POINT('Ctrl Pts',(-66.7175222527555,3.26438479979246,-2.70825681953606));
#42630=CARTESIAN_POINT('Ctrl Pts',(-66.5989901535054,4.16031329007191,-0.826230264593738));
#42631=CARTESIAN_POINT('Ctrl Pts',(-66.4804580542553,4.05154499755959,1.25532715035943));
#42632=CARTESIAN_POINT('Ctrl Pts',(-66.3619259550052,2.96434697137833,3.03372875434832));
#42633=CARTESIAN_POINT('Ctrl Pts',(-66.2433938557551,1.16127260186261,4.07949862922429));
#42634=CARTESIAN_POINT('Ctrl Pts',(-66.124861756505,-0.922243831912986,
4.14008809521949));
#42635=CARTESIAN_POINT('Ctrl Pts',(-66.006329657255,-2.78304256481646,3.20086507121113));
#42636=CARTESIAN_POINT('Ctrl Pts',(-65.8987715153953,-3.86169612693019,
1.64716843702214));
#42637=CARTESIAN_POINT('Ctrl Pts',(-65.8307240732857,-4.06994456648923,
0.486487869905523));
#42638=CARTESIAN_POINT('Ctrl Pts',(-65.8021873309261,-4.07040485551518,
-0.000100589830685713));
#42639=CARTESIAN_POINT('Origin',(-92.3478126690739,0.,0.));
#42640=CARTESIAN_POINT('',(-69.0978126690739,-4.07047413145155,-0.000103298102520897));
#42641=CARTESIAN_POINT('',(-68.8021873309261,-4.07020080396294,5.15392301635165E-5));
#42642=CARTESIAN_POINT('',(-92.3478126690739,-4.0705,-4.39132641279065E-13));
#42643=CARTESIAN_POINT('Ctrl Pts',(-69.0978126690739,-4.07047413145155,
-0.000103298102520806));
#42644=CARTESIAN_POINT('Ctrl Pts',(-69.0881907226276,-4.07063840498987,
-0.16416193285465));
#42645=CARTESIAN_POINT('Ctrl Pts',(-69.0390580764313,-4.0209408203763,-1.00179737554187));
#42646=CARTESIAN_POINT('Ctrl Pts',(-68.9504147304849,-3.45846662340299,
-2.45557970596334));
#42647=CARTESIAN_POINT('Ctrl Pts',(-68.8318826312348,-1.87113344337377,
-3.8065368400609));
#42648=CARTESIAN_POINT('Ctrl Pts',(-68.7133505319848,0.168069973265368,
-4.23823259881627));
#42649=CARTESIAN_POINT('Ctrl Pts',(-68.5948184327347,2.16668525394882,-3.64641441527627));
#42650=CARTESIAN_POINT('Ctrl Pts',(-68.4762863334845,3.64205587679515,-2.17400369546731));
#42651=CARTESIAN_POINT('Ctrl Pts',(-68.3577542342345,4.23788653064464,-0.176580947402252));
#42652=CARTESIAN_POINT('Ctrl Pts',(-68.2392221349844,3.81028681608063,1.86348529825389));
#42653=CARTESIAN_POINT('Ctrl Pts',(-68.1206900357343,2.46252012400403,3.45352829964948));
#42654=CARTESIAN_POINT('Ctrl Pts',(-68.0021579364842,0.520065995274375,
4.20955988651605));
#42655=CARTESIAN_POINT('Ctrl Pts',(-67.8836258372342,-1.54798171159727,
3.94900186099799));
#42656=CARTESIAN_POINT('Ctrl Pts',(-67.7650937379841,-3.24219885883922,
2.73477780401754));
#42657=CARTESIAN_POINT('Ctrl Pts',(-67.6698226819306,-3.97461545403881,
1.22800549874083));
#42658=CARTESIAN_POINT('Ctrl Pts',(-67.6140623256272,-4.07032877775755,
0.277169580906076));
#42659=CARTESIAN_POINT('Ctrl Pts',(-67.5978126690739,-4.07020210173435,
5.22794437558469E-5));
#42660=CARTESIAN_POINT('Ctrl Pts',(-68.8021873309261,-4.07020080396294,
5.15392301636899E-5));
#42661=CARTESIAN_POINT('Ctrl Pts',(-68.7789808672864,-4.07002252986222,
-0.395705654822888));
#42662=CARTESIAN_POINT('Ctrl Pts',(-68.7162637038966,-3.91510335891766,
-1.46540498961079));
#42663=CARTESIAN_POINT('Ctrl Pts',(-68.6140358407569,-2.99104255021837,
-3.00741210752073));
#42664=CARTESIAN_POINT('Ctrl Pts',(-68.4955037415068,-1.19728085404309,
-4.06907626842045));
#42665=CARTESIAN_POINT('Ctrl Pts',(-68.3769716422567,0.885618735911535,
-4.14807697328309));
#42666=CARTESIAN_POINT('Ctrl Pts',(-68.2584395430066,2.75464541949803,-3.22533591033841));
#42667=CARTESIAN_POINT('Ctrl Pts',(-68.1399074437565,3.9584377330416,-1.52369085949611));
#42668=CARTESIAN_POINT('Ctrl Pts',(-68.0213753445065,4.20628529483797,0.54591862040923));
#42669=CARTESIAN_POINT('Ctrl Pts',(-67.9028432452563,3.43833404328219,2.48369123050478));
#42670=CARTESIAN_POINT('Ctrl Pts',(-67.7843111460063,1.84004072116821,3.82166367778779));
#42671=CARTESIAN_POINT('Ctrl Pts',(-67.6657790467562,-0.202614086215485,
4.23672168707678));
#42672=CARTESIAN_POINT('Ctrl Pts',(-67.5472469475061,-2.19633851110734,
3.62863063238826));
#42673=CARTESIAN_POINT('Ctrl Pts',(-67.428714848256,-3.65965715110381,2.14424174431298));
#42674=CARTESIAN_POINT('Ctrl Pts',(-67.347028309396,-4.05903959952155,0.764413873298388));
#42675=CARTESIAN_POINT('Ctrl Pts',(-67.3048524702861,-4.07082728833475,
0.045476776836982));
#42676=CARTESIAN_POINT('Ctrl Pts',(-67.3021873309261,-4.07080131582391,
4.54689699825889E-5));
#42677=CARTESIAN_POINT('Origin',(-92.3478126690739,0.,0.));
#42678=CARTESIAN_POINT('',(-70.5978126690739,-4.07075375686348,6.52392274777287E-5));
#42679=CARTESIAN_POINT('',(-70.3021873309261,-4.07047700469628,-0.000103310864021655));
#42680=CARTESIAN_POINT('',(-92.3478126690739,-4.0705,-4.39132641279065E-13));
#42681=CARTESIAN_POINT('Ctrl Pts',(-70.5978126690739,-4.07075375686348,
6.52392274777796E-5));
#42682=CARTESIAN_POINT('Ctrl Pts',(-70.5623191196279,-4.07029028939964,
-0.604996165359999));
#42683=CARTESIAN_POINT('Ctrl Pts',(-70.4873148704319,-3.78140816801703,
-1.88402768221452));
#42684=CARTESIAN_POINT('Ctrl Pts',(-70.372799921486,-2.49294537375558,-3.43163023054535));
#42685=CARTESIAN_POINT('Ctrl Pts',(-70.2542678222358,-0.557248744408297,
-4.20479929705468));
#42686=CARTESIAN_POINT('Ctrl Pts',(-70.1357357229858,1.51302095431612,-3.96252830672392));
#42687=CARTESIAN_POINT('Ctrl Pts',(-70.0172036237356,3.21790294474063,-2.7633247619019));
#42688=CARTESIAN_POINT('Ctrl Pts',(-69.8986715244856,4.14567598115117,-0.896790799288985));
#42689=CARTESIAN_POINT('Ctrl Pts',(-69.7801394252355,4.07228707527332,1.18631405942714));
#42690=CARTESIAN_POINT('Ctrl Pts',(-69.6616073259855,3.01545931965475,2.98292946189813));
#42691=CARTESIAN_POINT('Ctrl Pts',(-69.5430752267353,1.23041181972154,4.05918093071395));
#42692=CARTESIAN_POINT('Ctrl Pts',(-69.4245431274853,-0.851774551486206,
4.15515862422754));
#42693=CARTESIAN_POINT('Ctrl Pts',(-69.3060110282352,-2.72826123349541,
3.24768436257942));
#42694=CARTESIAN_POINT('Ctrl Pts',(-69.1971008754314,-3.84704351951115,
1.69324039772707));
#42695=CARTESIAN_POINT('Ctrl Pts',(-69.1277014223776,-4.06996384683415,
0.509513762107668));
#42696=CARTESIAN_POINT('Ctrl Pts',(-69.0978126690739,-4.07047413145155,
-0.000103298102520806));
#42697=CARTESIAN_POINT('Ctrl Pts',(-70.3021873309261,-4.07047700469628,
-0.000103310864021447));
#42698=CARTESIAN_POINT('Ctrl Pts',(-70.2926199640367,-4.0706405847988,-0.163231007798239));
#42699=CARTESIAN_POINT('Ctrl Pts',(-70.2435418973974,-4.02128126826631,
-0.999934669155785));
#42700=CARTESIAN_POINT('Ctrl Pts',(-70.154953131008,-3.46015001328113,-2.45320708625443));
#42701=CARTESIAN_POINT('Ctrl Pts',(-70.0364210317579,-1.87374378398806,
-3.80525259964336));
#42702=CARTESIAN_POINT('Ctrl Pts',(-69.9178889325078,0.165163070961228,
-4.23834688141492));
#42703=CARTESIAN_POINT('Ctrl Pts',(-69.7993568332577,2.16418379186852,-3.64789961943599));
#42704=CARTESIAN_POINT('Ctrl Pts',(-69.6808247340076,3.64056394757633,-2.17650115247581));
#42705=CARTESIAN_POINT('Ctrl Pts',(-69.5622926347575,4.2377644279798,-0.179487532051847));
#42706=CARTESIAN_POINT('Ctrl Pts',(-69.4437605355075,3.81156402742994,1.8608715126343));
#42707=CARTESIAN_POINT('Ctrl Pts',(-69.3252284362573,2.46488820851225,3.45183853059299));
#42708=CARTESIAN_POINT('Ctrl Pts',(-69.2066963370073,0.522953071331976,
4.20920220550053));
#42709=CARTESIAN_POINT('Ctrl Pts',(-69.0881642377572,-1.54527285978556,
3.95006264640662));
#42710=CARTESIAN_POINT('Ctrl Pts',(-68.9696321385071,-3.24032240668157,
2.737000880967));
#42711=CARTESIAN_POINT('Ctrl Pts',(-68.8743065028967,-3.97419245969456,
1.22986834614377));
#42712=CARTESIAN_POINT('Ctrl Pts',(-68.8184915670364,-4.07032605454294,
0.278099881035541));
#42713=CARTESIAN_POINT('Ctrl Pts',(-68.8021873309261,-4.07020080396294,
5.15392301636899E-5));
#42714=CARTESIAN_POINT('Origin',(-92.3478126690739,0.,0.));
#42715=CARTESIAN_POINT('',(-72.0978126690739,-4.07028079851592,-0.000396239704358614));
#42716=CARTESIAN_POINT('',(-71.8021873309261,-4.07074215327807,5.17293523791262E-5));
#42717=CARTESIAN_POINT('',(-92.3478126690739,-4.0705,-4.39132641279065E-13));
#42718=CARTESIAN_POINT('Ctrl Pts',(-72.0978126690739,-4.07028079851592,
-0.000396239704358523));
#42719=CARTESIAN_POINT('Ctrl Pts',(-72.0759582163783,-4.07012861038251,
-0.3729091594408));
#42720=CARTESIAN_POINT('Ctrl Pts',(-72.0145930639327,-3.92738889203425,
-1.41858141393639));
#42721=CARTESIAN_POINT('Ctrl Pts',(-71.9137172117371,-3.04181408411095,
-2.95660822043184));
#42722=CARTESIAN_POINT('Ctrl Pts',(-71.7951851124869,-1.26618312449043,
-4.04792730165813));
#42723=CARTESIAN_POINT('Ctrl Pts',(-71.676653013237,0.814991865508356,-4.1626338697688));
#42724=CARTESIAN_POINT('Ctrl Pts',(-71.5581209139868,2.69946593220966,-3.27161473710967));
#42725=CARTESIAN_POINT('Ctrl Pts',(-71.4395888147368,3.93197366980717,-1.59074811823812));
#42726=CARTESIAN_POINT('Ctrl Pts',(-71.3210567154866,4.21495618453984,0.474392460257583));
#42727=CARTESIAN_POINT('Ctrl Pts',(-71.2025246162366,3.48003171573737,2.42491205953816));
#42728=CARTESIAN_POINT('Ctrl Pts',(-71.0839925169865,1.90470242326041,3.78985487631873));
#42729=CARTESIAN_POINT('Ctrl Pts',(-70.9654604177364,-0.130607360489598,
4.2395507965525));
#42730=CARTESIAN_POINT('Ctrl Pts',(-70.8469283184863,-2.13437432226263,
3.6654214565239));
#42731=CARTESIAN_POINT('Ctrl Pts',(-70.7283962192362,-3.62270043207957,
2.20610597997014));
#42732=CARTESIAN_POINT('Ctrl Pts',(-70.6453576694321,-4.05246440445107,
0.810540587465255));
#42733=CARTESIAN_POINT('Ctrl Pts',(-70.601829819378,-4.07080621198539,0.068545924968227));
#42734=CARTESIAN_POINT('Ctrl Pts',(-70.5978126690739,-4.07075375686348,
6.52392274777796E-5));
#42735=CARTESIAN_POINT('Ctrl Pts',(-71.8021873309261,-4.07074215327807,
5.17293523791609E-5));
#42736=CARTESIAN_POINT('Ctrl Pts',(-71.7667483610371,-4.07027236134414,
-0.6040848204387));
#42737=CARTESIAN_POINT('Ctrl Pts',(-71.6917986913982,-3.78210048234303,
-1.88214965493016));
#42738=CARTESIAN_POINT('Ctrl Pts',(-71.5773383220089,-2.49529078987354,
-3.42993115267771));
#42739=CARTESIAN_POINT('Ctrl Pts',(-71.458806222759,-0.560136340693826,
-4.20441037867915));
#42740=CARTESIAN_POINT('Ctrl Pts',(-71.3402741235088,1.5103047169698,-3.96356795830934));
#42741=CARTESIAN_POINT('Ctrl Pts',(-71.2217420242588,3.21600598369556,-2.76552975458416));
#42742=CARTESIAN_POINT('Ctrl Pts',(-71.1032099250086,4.14506039630085,-0.899634673257719));
#42743=CARTESIAN_POINT('Ctrl Pts',(-70.9846778257586,4.07309954546553,1.18352108347017));
#42744=CARTESIAN_POINT('Ctrl Pts',(-70.8661457265085,3.01750462107274,2.98086038723955));
#42745=CARTESIAN_POINT('Ctrl Pts',(-70.7476136272584,1.23319553280523,4.0583361681078));
#42746=CARTESIAN_POINT('Ctrl Pts',(-70.6290815280083,-0.848924438267781,
4.15574181331312));
#42747=CARTESIAN_POINT('Ctrl Pts',(-70.5105494287582,-2.72603312996977,
3.24955484789199));
#42748=CARTESIAN_POINT('Ctrl Pts',(-70.4015846963975,-3.84644248062139,
1.69509993942009));
#42749=CARTESIAN_POINT('Ctrl Pts',(-70.3321306637868,-4.0699650421557,0.51044331963423));
#42750=CARTESIAN_POINT('Ctrl Pts',(-70.3021873309261,-4.07047700469628,
-0.000103310864021447));
#42751=CARTESIAN_POINT('Origin',(-92.3478126690739,0.,0.));
#42752=CARTESIAN_POINT('',(-73.5978126690739,-4.06507175003265,0.00203090272800402));
#42753=CARTESIAN_POINT('',(-73.3021873309261,-4.06969892170118,-0.00325965976725018));
#42754=CARTESIAN_POINT('',(-92.3478126690739,-4.0705,-4.39132641279065E-13));
#42755=CARTESIAN_POINT('Ctrl Pts',(-73.5978126690739,-4.06507175003265,
0.00203090272800382));
#42756=CARTESIAN_POINT('Ctrl Pts',(-73.5500866133787,-4.06112590042124,
-0.814333197936782));
#42757=CARTESIAN_POINT('Ctrl Pts',(-73.4233391581834,-3.42780995393646,
-2.98789524608297));
#42758=CARTESIAN_POINT('Ctrl Pts',(-73.217570303488,0.104851279587011,-4.80118117413053));
#42759=CARTESIAN_POINT('Ctrl Pts',(-72.9805061049878,4.0818527109764,-2.5374258400941));
#42760=CARTESIAN_POINT('Ctrl Pts',(-72.7434419064878,4.34947338571156,2.0393426803231));
#42761=CARTESIAN_POINT('Ctrl Pts',(-72.5458884077375,1.29059508521834,4.29352941894811));
#42762=CARTESIAN_POINT('Ctrl Pts',(-72.3878456087375,-1.47975600101921,
3.96853832825987));
#42763=CARTESIAN_POINT('Ctrl Pts',(-72.2693135094873,-3.19245598996507,
2.7952829416349));
#42764=CARTESIAN_POINT('Ctrl Pts',(-72.1726358629329,-3.96369324348151,
1.2752093510444));
#42765=CARTESIAN_POINT('Ctrl Pts',(-72.1154689161283,-4.0704037515507,0.300557539988409));
#42766=CARTESIAN_POINT('Ctrl Pts',(-72.0978126690739,-4.07028079851592,
-0.000396239704358523));
#42767=CARTESIAN_POINT('Ctrl Pts',(-73.3021873309261,-4.06969892170118,
-0.00325965976725035));
#42768=CARTESIAN_POINT('Ctrl Pts',(-73.2803874577875,-4.072936090382,-0.375222354381865));
#42769=CARTESIAN_POINT('Ctrl Pts',(-73.1795661851488,-3.85606008990605,
-2.09201308027041));
#42770=CARTESIAN_POINT('Ctrl Pts',(-72.9997235130101,-1.43150958571139,
-4.58558645780951));
#42771=CARTESIAN_POINT('Ctrl Pts',(-72.8021700142599,2.29645120176649,-3.85049572963833));
#42772=CARTESIAN_POINT('Ctrl Pts',(-72.6441272152598,3.92679810234926,-1.58721605638371));
#42773=CARTESIAN_POINT('Ctrl Pts',(-72.5255951160097,4.21734429791554,0.468377299721421));
#42774=CARTESIAN_POINT('Ctrl Pts',(-72.4070630167596,3.4806665638518,2.42407836288371));
#42775=CARTESIAN_POINT('Ctrl Pts',(-72.2885309175095,1.90781163232082,3.78777607431905));
#42776=CARTESIAN_POINT('Ctrl Pts',(-72.1699988182595,-0.127952933172336,
4.24002244278688));
#42777=CARTESIAN_POINT('Ctrl Pts',(-72.0514667190093,-2.13173404035006,
3.66669431825119));
#42778=CARTESIAN_POINT('Ctrl Pts',(-71.9329346197594,-3.62124894073959,
2.20868457101181));
#42779=CARTESIAN_POINT('Ctrl Pts',(-71.8498414903981,-4.05218757424346,
0.812398134823304));
#42780=CARTESIAN_POINT('Ctrl Pts',(-71.8062590607871,-4.07079612961688,
0.0694634768615688));
#42781=CARTESIAN_POINT('Ctrl Pts',(-71.8021873309261,-4.07074215327807,
5.17293523791609E-5));
#42782=CARTESIAN_POINT('Origin',(-92.3478126690739,0.,0.));
#42783=CARTESIAN_POINT('',(-75.0978126690739,-4.07583767183017,0.00141285829539006));
#42784=CARTESIAN_POINT('',(-74.8021873309261,-4.06510912917479,0.00214260453011594));
#42785=CARTESIAN_POINT('',(-92.3478126690739,-4.0705,-4.39132641279065E-13));
#42786=CARTESIAN_POINT('Ctrl Pts',(-75.0978126690739,-4.07583767183017,
0.00141285829539012));
#42787=CARTESIAN_POINT('Ctrl Pts',(-75.024215010379,-4.06930339312292,-1.24860930367453));
#42788=CARTESIAN_POINT('Ctrl Pts',(-74.8715959521841,-2.78876718547004,
-3.85121310504378));
#42789=CARTESIAN_POINT('Ctrl Pts',(-74.639955494489,1.63433374823429,-4.51748027493275));
#42790=CARTESIAN_POINT('Ctrl Pts',(-74.402891295989,4.6763033020638,-1.09843764222045));
#42791=CARTESIAN_POINT('Ctrl Pts',(-74.1658270974887,3.47436957665643,3.31745869645859));
#42792=CARTESIAN_POINT('Ctrl Pts',(-73.9287628989886,-0.881308697829502,
4.72204116943823));
#42793=CARTESIAN_POINT('Ctrl Pts',(-73.7394247561836,-3.72131169761533,
2.42118440488785));
#42794=CARTESIAN_POINT('Ctrl Pts',(-73.6291080128787,-4.0676591568148,0.537344262025627));
#42795=CARTESIAN_POINT('Ctrl Pts',(-73.5978126690739,-4.06507175003265,
0.00203090272800382));
#42796=CARTESIAN_POINT('Ctrl Pts',(-74.8021873309261,-4.06510912917479,
0.00214260453011594));
#42797=CARTESIAN_POINT('Ctrl Pts',(-74.7545158547878,-4.06124659588267,
-0.813195354839492));
#42798=CARTESIAN_POINT('Ctrl Pts',(-74.6278229791496,-3.42914710515804,
-2.98561629200826));
#42799=CARTESIAN_POINT('Ctrl Pts',(-74.422108704011,0.102291553945791,-4.80267280759255));
#42800=CARTESIAN_POINT('Ctrl Pts',(-74.185044505511,4.07867853910156,-2.53741907084073));
#42801=CARTESIAN_POINT('Ctrl Pts',(-73.9479803070107,4.35373227228281,2.03076696083007));
#42802=CARTESIAN_POINT('Ctrl Pts',(-73.7109161085106,0.675669024164784,
4.75614017541162));
#42803=CARTESIAN_POINT('Ctrl Pts',(-73.4956517831491,-3.21859608763278,
3.31010339667926));
#42804=CARTESIAN_POINT('Ctrl Pts',(-73.3594088572876,-4.06120182028099,
0.973088826299921));
#42805=CARTESIAN_POINT('Ctrl Pts',(-73.3021873309261,-4.06969892170118,
-0.00325965976725035));
#42806=CARTESIAN_POINT('Origin',(-92.3478126690739,0.,0.));
#42807=CARTESIAN_POINT('',(-76.5978126690739,-4.07011789117663,1.93561709038092E-5));
#42808=CARTESIAN_POINT('',(-76.3021873309261,-4.07616962263128,0.0032098901687027));
#42809=CARTESIAN_POINT('',(-92.3478126690739,-4.0705,-4.39132641279065E-13));
#42810=CARTESIAN_POINT('Ctrl Pts',(-76.5978126690739,-4.07011789117663,
1.93561709039766E-5));
#42811=CARTESIAN_POINT('Ctrl Pts',(-76.5773648068794,-4.07005952701129,
-0.348697968315602));
#42812=CARTESIAN_POINT('Ctrl Pts',(-76.5174062449349,-3.93994663469226,
-1.3712594731013));
#42813=CARTESIAN_POINT('Ctrl Pts',(-76.4179369832404,-3.09392819414575,
-2.90202919022035));
#42814=CARTESIAN_POINT('Ctrl Pts',(-76.2994048839903,-1.33668453718049,
-4.02495526764412));
#42815=CARTESIAN_POINT('Ctrl Pts',(-76.1808727847402,0.739496217920181,
-4.17664208939481));
#42816=CARTESIAN_POINT('Ctrl Pts',(-76.0623406854901,2.64486935815373,-3.3181392451129));
#42817=CARTESIAN_POINT('Ctrl Pts',(-75.9438085862401,3.89596740984592,-1.66144883365045));
#42818=CARTESIAN_POINT('Ctrl Pts',(-75.7857657872398,4.3485497237372,1.09093805761265));
#42819=CARTESIAN_POINT('Ctrl Pts',(-75.5882122884899,2.2380304938709,4.25065369199898));
#42820=CARTESIAN_POINT('Ctrl Pts',(-75.3511480899896,-2.34621401747439,
4.19467891885534));
#42821=CARTESIAN_POINT('Ctrl Pts',(-75.1876815501843,-4.03215439766421,
1.5273685129187));
#42822=CARTESIAN_POINT('Ctrl Pts',(-75.1032364098791,-4.0763192120678,0.0935325850297277));
#42823=CARTESIAN_POINT('Ctrl Pts',(-75.0978126690739,-4.07583767183017,
0.00141285829539012));
#42824=CARTESIAN_POINT('Ctrl Pts',(-76.3021873309261,-4.07616962263128,
0.00320989016870294));
#42825=CARTESIAN_POINT('Ctrl Pts',(-76.2286442517882,-4.0696862238209,-1.24479614250474));
#42826=CARTESIAN_POINT('Ctrl Pts',(-76.0760797731501,-2.78983322256644,
-3.85270151269288));
#42827=CARTESIAN_POINT('Ctrl Pts',(-75.8444938950122,1.63095801340486,-4.51688897627564));
#42828=CARTESIAN_POINT('Ctrl Pts',(-75.607429696512,4.67567242759371,-1.10249052069397));
#42829=CARTESIAN_POINT('Ctrl Pts',(-75.3703654980118,3.47661902182452,3.31543652103366));
#42830=CARTESIAN_POINT('Ctrl Pts',(-75.1333012995117,-0.878131813745364,
4.72260507390595));
#42831=CARTESIAN_POINT('Ctrl Pts',(-74.9439085771497,-3.72034050812532,
2.4228541118301));
#42832=CARTESIAN_POINT('Ctrl Pts',(-74.8335372542879,-4.06764922510844,
0.538328697573246));
#42833=CARTESIAN_POINT('Ctrl Pts',(-74.8021873309261,-4.06510912917479,
0.00214260453011594));
#42834=CARTESIAN_POINT('Origin',(-92.3478126690739,0.,0.));
#42835=CARTESIAN_POINT('',(-78.0978126690738,-4.07062303909154,-9.39073287783277E-5));
#42836=CARTESIAN_POINT('',(-77.8021873309261,-4.07016223393827,1.2136666346918E-5));
#42837=CARTESIAN_POINT('',(-92.3478126690739,-4.0705,-4.39132641279065E-13));
#42838=CARTESIAN_POINT('Ctrl Pts',(-78.0978126690738,-4.07062303909154,
-9.39073287782588E-5));
#42839=CARTESIAN_POINT('Ctrl Pts',(-78.0910039036297,-4.07073767756003,
-0.116174268661055));
#42840=CARTESIAN_POINT('Ctrl Pts',(-78.0446844384356,-4.03762736234282,
-0.905794127161616));
#42841=CARTESIAN_POINT('Ctrl Pts',(-77.9588542734915,-3.54309601390001,
-2.33180902134115));
#42842=CARTESIAN_POINT('Ctrl Pts',(-77.8403221742414,-2.00450312872445,
-3.73802499184148));
#42843=CARTESIAN_POINT('Ctrl Pts',(-77.7217900749913,0.0181685980883059,
-4.2415248017455));
#42844=CARTESIAN_POINT('Ctrl Pts',(-77.6032579757413,2.03645182254301,-3.72071578999402));
#42845=CARTESIAN_POINT('Ctrl Pts',(-77.4847258764911,3.56294292078298,-2.30137044925895));
#42846=CARTESIAN_POINT('Ctrl Pts',(-77.3661937772411,4.22899594778787,-0.326255287706977));
#42847=CARTESIAN_POINT('Ctrl Pts',(-77.247661677991,3.87377273534343,1.72765045644101));
#42848=CARTESIAN_POINT('Ctrl Pts',(-77.1291295787409,2.58303669769032,3.36433361268123));
#42849=CARTESIAN_POINT('Ctrl Pts',(-77.0105974794908,0.668537789879148,
4.18855118954554));
#42850=CARTESIAN_POINT('Ctrl Pts',(-76.8920653802408,-1.40746790745146,
4.00124113310223));
#42851=CARTESIAN_POINT('Ctrl Pts',(-76.7735332809906,-3.14345978794428,
2.84767271097138));
#42852=CARTESIAN_POINT('Ctrl Pts',(-76.6754490439351,-3.95199757018475,
1.32400107408212));
#42853=CARTESIAN_POINT('Ctrl Pts',(-76.6168755066295,-4.07017230207751,
0.325116505509737));
#42854=CARTESIAN_POINT('Ctrl Pts',(-76.5978126690739,-4.07011789117663,
1.93561709039766E-5));
#42855=CARTESIAN_POINT('Ctrl Pts',(-77.8021873309261,-4.07016223393827,
1.21366663470221E-5));
#42856=CARTESIAN_POINT('Ctrl Pts',(-77.7817940482886,-4.07013329270246,
-0.347778280513504));
#42857=CARTESIAN_POINT('Ctrl Pts',(-77.721890065901,-3.94054142339228,-1.36941406884846));
#42858=CARTESIAN_POINT('Ctrl Pts',(-77.6224753837634,-3.09545209551088,
-2.89984013449786));
#42859=CARTESIAN_POINT('Ctrl Pts',(-77.5039432845133,-1.34038284556851,
-4.02417116971747));
#42860=CARTESIAN_POINT('Ctrl Pts',(-77.3854111852633,0.738520086648723,
-4.17687915873197));
#42861=CARTESIAN_POINT('Ctrl Pts',(-77.2668790860131,2.63879720128349,-3.32049492888954));
#42862=CARTESIAN_POINT('Ctrl Pts',(-77.1483469867632,3.90237383473824,-1.66302156401962));
#42863=CARTESIAN_POINT('Ctrl Pts',(-77.0298148875129,4.22242284177216,0.397665888508434));
#42864=CARTESIAN_POINT('Ctrl Pts',(-76.911282788263,3.52503575024894,2.35909274883029));
#42865=CARTESIAN_POINT('Ctrl Pts',(-76.7927506890127,1.97181984252191,3.75729912712469));
#42866=CARTESIAN_POINT('Ctrl Pts',(-76.6742185897627,-0.0484579238967644,
4.23516823465935));
#42867=CARTESIAN_POINT('Ctrl Pts',(-76.5161757907627,-2.75000559908163,
3.54082966140385));
#42868=CARTESIAN_POINT('Ctrl Pts',(-76.3921653711505,-4.03185271297995,
1.52933182071804));
#42869=CARTESIAN_POINT('Ctrl Pts',(-76.3076656512883,-4.07665257950683,
0.0961754953757293));
#42870=CARTESIAN_POINT('Ctrl Pts',(-76.3021873309261,-4.07616962263128,
0.00320989016870294));
#42871=CARTESIAN_POINT('Origin',(-92.3478126690739,0.,0.));
#42872=CARTESIAN_POINT('',(-79.5978126690739,-4.07062191593116,9.40553201711143E-5));
#42873=CARTESIAN_POINT('',(-79.3021873309261,-4.07062585394818,-9.35223854153788E-5));
#42874=CARTESIAN_POINT('',(-92.3478126690739,-4.0705,-4.39132641279065E-13));
#42875=CARTESIAN_POINT('Ctrl Pts',(-79.5978126690739,-4.07062191593116,
9.40553201713226E-5));
#42876=CARTESIAN_POINT('Ctrl Pts',(-79.5651323006301,-4.07007120518726,
-0.557063040139934));
#42877=CARTESIAN_POINT('Ctrl Pts',(-79.4929412324364,-3.81534586386885,
-1.78831340922059));
#42878=CARTESIAN_POINT('Ctrl Pts',(-79.3812394644925,-2.61267572378093,
-3.34137526175934));
#42879=CARTESIAN_POINT('Ctrl Pts',(-79.2627073652425,-0.705515467763387,
-4.18247665892133));
#42880=CARTESIAN_POINT('Ctrl Pts',(-79.1441752659924,1.3720235726515,-4.01352892025788));
#42881=CARTESIAN_POINT('Ctrl Pts',(-79.0256431667423,3.11822514541502,-2.87533215814075));
#42882=CARTESIAN_POINT('Ctrl Pts',(-78.9071110674922,4.11138949440471,-1.04275572611736));
#42883=CARTESIAN_POINT('Ctrl Pts',(-78.7885789682421,4.11167193448134,1.04164148226761));
#42884=CARTESIAN_POINT('Ctrl Pts',(-78.670046868992,3.11900426003185,2.87448699928452));
#42885=CARTESIAN_POINT('Ctrl Pts',(-78.551514769742,1.37311120556277,4.01315694786418));
#42886=CARTESIAN_POINT('Ctrl Pts',(-78.4329826704918,-0.704381968314586,
4.18266770388186));
#42887=CARTESIAN_POINT('Ctrl Pts',(-78.3144505712418,-2.61177010587796,
3.34208318501393));
#42888=CARTESIAN_POINT('Ctrl Pts',(-78.2027272374358,-3.81509334776075,
1.78904754094927));
#42889=CARTESIAN_POINT('Ctrl Pts',(-78.1305146033798,-4.0700724400591,0.557430416525206));
#42890=CARTESIAN_POINT('Ctrl Pts',(-78.0978126690738,-4.07062303909154,
-9.39073287782588E-5));
#42891=CARTESIAN_POINT('Ctrl Pts',(-79.3021873309261,-4.07062585394818,
-9.35223854152401E-5));
#42892=CARTESIAN_POINT('Ctrl Pts',(-79.295433145039,-4.0707393191523,-0.115243145155149));
#42893=CARTESIAN_POINT('Ctrl Pts',(-79.2491682594018,-4.03793381614542,
-0.903931660617922));
#42894=CARTESIAN_POINT('Ctrl Pts',(-79.1633926740146,-3.54469454740893,
-2.32937839090772));
#42895=CARTESIAN_POINT('Ctrl Pts',(-79.0448605747645,-2.00706634268101,
-3.73664927998142));
#42896=CARTESIAN_POINT('Ctrl Pts',(-78.9263284755144,0.0152592617744791,
-4.24153630056935));
#42897=CARTESIAN_POINT('Ctrl Pts',(-78.8077963762643,2.03389985453592,-3.72211159382277));
#42898=CARTESIAN_POINT('Ctrl Pts',(-78.6892642770142,3.56136279891019,-2.30381373712066));
#42899=CARTESIAN_POINT('Ctrl Pts',(-78.5707321777641,4.22877291137641,-0.329155494427314));
#42900=CARTESIAN_POINT('Ctrl Pts',(-78.4522000785141,3.87495330153115,1.72499266588648));
#42901=CARTESIAN_POINT('Ctrl Pts',(-78.333667979264,2.58535055813011,3.36256220074308));
#42902=CARTESIAN_POINT('Ctrl Pts',(-78.2151358800139,0.671396364788188,
4.18808967855972));
#42903=CARTESIAN_POINT('Ctrl Pts',(-78.0966037807638,-1.40469494822981,
4.00220956636128));
#42904=CARTESIAN_POINT('Ctrl Pts',(-77.9780716815137,-3.14156294622147,
2.84981991591854));
#42905=CARTESIAN_POINT('Ctrl Pts',(-77.8799328649011,-3.95145378701792,
1.32587590907784));
#42906=CARTESIAN_POINT('Ctrl Pts',(-77.8213047480386,-4.07018936452272,
0.326043732027068));
#42907=CARTESIAN_POINT('Ctrl Pts',(-77.8021873309261,-4.07016223393827,
1.21366663470221E-5));
#42908=CARTESIAN_POINT('Origin',(-92.3478126690739,0.,0.));
#42909=CARTESIAN_POINT('',(-81.0978126690739,-4.07016105732122,-1.11263490865075E-5));
#42910=CARTESIAN_POINT('',(-80.8021873309261,-4.07061909410162,9.44285938865585E-5));
#42911=CARTESIAN_POINT('',(-92.3478126690739,-4.0705,-4.39132641279065E-13));
#42912=CARTESIAN_POINT('Ctrl Pts',(-81.0978126690739,-4.07016105732122,
-1.11263490864752E-5));
#42913=CARTESIAN_POINT('Ctrl Pts',(-81.0787713973805,-4.07019225222942,
-0.324745259963735));
#42914=CARTESIAN_POINT('Ctrl Pts',(-81.020219425937,-3.95209632995797,-1.3232814526723));
#42915=CARTESIAN_POINT('Ctrl Pts',(-80.9221567547438,-3.14428645876529,
-2.84680974826745));
#42916=CARTESIAN_POINT('Ctrl Pts',(-80.8036246554935,-1.40852487473531,
-4.00086500082885));
#42917=CARTESIAN_POINT('Ctrl Pts',(-80.6850925562435,0.667389075585396,
-4.18872950897938));
#42918=CARTESIAN_POINT('Ctrl Pts',(-80.5665604569934,2.58213159232414,-3.36503484640604));
#42919=CARTESIAN_POINT('Ctrl Pts',(-80.4480283577433,3.87330104552845,-1.72869953673665));
#42920=CARTESIAN_POINT('Ctrl Pts',(-80.3294962584933,4.22908587072581,0.325108867355182));
#42921=CARTESIAN_POINT('Ctrl Pts',(-80.2109641592431,3.56356564694796,2.30040495511053));
#42922=CARTESIAN_POINT('Ctrl Pts',(-80.0924320599931,2.03746048854546,3.72016368392876));
#42923=CARTESIAN_POINT('Ctrl Pts',(-79.9738999607429,0.0193178668117769,
4.2415197627297));
#42924=CARTESIAN_POINT('Ctrl Pts',(-79.855367861493,-2.00348993210374,3.73856806405375));
#42925=CARTESIAN_POINT('Ctrl Pts',(-79.7368357622428,-3.54246400293638,
2.33276914106685));
#42926=CARTESIAN_POINT('Ctrl Pts',(-79.6509840314364,-4.03750608952868,
0.906530038982288));
#42927=CARTESIAN_POINT('Ctrl Pts',(-79.6046430003801,-4.07073701673981,
0.116542177935112));
#42928=CARTESIAN_POINT('Ctrl Pts',(-79.5978126690739,-4.07062191593116,
9.40553201713226E-5));
#42929=CARTESIAN_POINT('Ctrl Pts',(-80.8021873309261,-4.07061909410162,
9.44285938865412E-5));
#42930=CARTESIAN_POINT('Ctrl Pts',(-80.7695615420393,-4.07006813553142,
-0.556133273234639));
#42931=CARTESIAN_POINT('Ctrl Pts',(-80.6974250534025,-3.81598438975405,
-1.78645542910972));
#42932=CARTESIAN_POINT('Ctrl Pts',(-80.5857778650156,-2.61496685112479,
-3.33958253217321));
#42933=CARTESIAN_POINT('Ctrl Pts',(-80.4672457657655,-0.708383924910281,
-4.18199179059653));
#42934=CARTESIAN_POINT('Ctrl Pts',(-80.3487136665154,1.36927050498713,-4.01446900670923));
#42935=CARTESIAN_POINT('Ctrl Pts',(-80.2301815672654,3.11625232078442,-2.87747017272681));
#42936=CARTESIAN_POINT('Ctrl Pts',(-80.1116494680153,4.11067334059816,-1.04557534807476));
#42937=CARTESIAN_POINT('Ctrl Pts',(-79.9931173687652,4.11238540021266,1.03882117896535));
#42938=CARTESIAN_POINT('Ctrl Pts',(-79.8745852695151,3.12097504491475,2.87234710485192));
#42939=CARTESIAN_POINT('Ctrl Pts',(-79.756053170265,1.37586337731199,4.01221423757314));
#42940=CARTESIAN_POINT('Ctrl Pts',(-79.6375210710149,-0.701513053379031,
4.18314983703188));
#42941=CARTESIAN_POINT('Ctrl Pts',(-79.5189889717648,-2.60947726422201,
3.343873730567));
#42942=CARTESIAN_POINT('Ctrl Pts',(-79.4072110584019,-3.81445379114245,
1.79090547468083));
#42943=CARTESIAN_POINT('Ctrl Pts',(-79.334943844789,-4.07007556934039,0.558360194698833));
#42944=CARTESIAN_POINT('Ctrl Pts',(-79.3021873309261,-4.07062585394818,
-9.35223854152401E-5));
#42945=CARTESIAN_POINT('Origin',(-92.3478126690739,0.,0.));
#42946=CARTESIAN_POINT('',(-82.5978126690739,-4.07069297892822,-8.16732152922881E-5));
#42947=CARTESIAN_POINT('',(-82.3021873309261,-4.07016134870022,-1.19732118704363E-5));
#42948=CARTESIAN_POINT('',(-92.3478126690739,-4.0705,-4.39132641279065E-13));
#42949=CARTESIAN_POINT('Ctrl Pts',(-82.5978126690739,-4.07069297892822,
-8.16732152923022E-5));
#42950=CARTESIAN_POINT('Ctrl Pts',(-82.5924104941309,-4.07077627717628,
-0.0921769713394929));
#42951=CARTESIAN_POINT('Ctrl Pts',(-82.5474976194379,-4.04531628661873,
-0.857797526681112));
#42952=CARTESIAN_POINT('Ctrl Pts',(-82.4630740449948,-3.58375688894285,
-2.26882120021829));
#42953=CARTESIAN_POINT('Ctrl Pts',(-82.3445419457447,-2.0702588085909,-3.70201182373276));
#42954=CARTESIAN_POINT('Ctrl Pts',(-82.2260098464947,-0.0568026194346637,
-4.24118338910624));
#42955=CARTESIAN_POINT('Ctrl Pts',(-82.1074777472446,1.97037114458219,-3.75612840970636));
#42956=CARTESIAN_POINT('Ctrl Pts',(-81.9889456479944,3.52170921742845,-2.36398546219828));
#42957=CARTESIAN_POINT('Ctrl Pts',(-81.8704135487444,4.2225704934618,-0.40095075177776));
#42958=CARTESIAN_POINT('Ctrl Pts',(-81.7518814494942,3.90370015456685,1.65891174594675));
#42959=CARTESIAN_POINT('Ctrl Pts',(-81.6333493502442,2.64210394076326,3.31815458407359));
#42960=CARTESIAN_POINT('Ctrl Pts',(-81.514817250994,0.742451613392211,4.17607814574591));
#42961=CARTESIAN_POINT('Ctrl Pts',(-81.3962851517442,-1.33649940985683,
4.02549778351171));
#42962=CARTESIAN_POINT('Ctrl Pts',(-81.2777530524938,-3.09269188977919,
2.90277797161605));
#42963=CARTESIAN_POINT('Ctrl Pts',(-81.1782622249373,-3.93987357385575,
1.37201827475063));
#42964=CARTESIAN_POINT('Ctrl Pts',(-81.1182820971305,-4.07012752269499,
0.349079107360558));
#42965=CARTESIAN_POINT('Ctrl Pts',(-81.0978126690739,-4.07016105732122,
-1.11263490864752E-5));
#42966=CARTESIAN_POINT('Ctrl Pts',(-82.3021873309261,-4.07016134870022,
-1.1973211870471E-5));
#42967=CARTESIAN_POINT('Ctrl Pts',(-82.2832006387897,-4.07019482461848,
-0.323815229975626));
#42968=CARTESIAN_POINT('Ctrl Pts',(-82.2247032469032,-3.95255397240321,
-1.3214188020348));
#42969=CARTESIAN_POINT('Ctrl Pts',(-82.1266951552668,-3.14623825560085,
-2.84465252019879));
#42970=CARTESIAN_POINT('Ctrl Pts',(-82.0081630560165,-1.41126860599162,
-3.99989800412737));
#42971=CARTESIAN_POINT('Ctrl Pts',(-81.8896309567667,0.664516008557521,
-4.18918626896089));
#42972=CARTESIAN_POINT('Ctrl Pts',(-81.7710988575164,2.57982302217583,-3.36680505760746));
#42973=CARTESIAN_POINT('Ctrl Pts',(-81.6525667582664,3.87211448147575,-1.73135570118489));
#42974=CARTESIAN_POINT('Ctrl Pts',(-81.5340346590163,4.22930786260355,0.322208201322427));
#42975=CARTESIAN_POINT('Ctrl Pts',(-81.4155025597663,3.56514258472508,2.29796028517889));
#42976=CARTESIAN_POINT('Ctrl Pts',(-81.2969704605161,2.04001154890355,3.71876538679436));
#42977=CARTESIAN_POINT('Ctrl Pts',(-81.178438361266,0.0222269802501248,
4.24150552080608));
#42978=CARTESIAN_POINT('Ctrl Pts',(-81.0599062620159,-2.00092530328236,
3.73994131670062));
#42979=CARTESIAN_POINT('Ctrl Pts',(-80.9413741627659,-3.54086320495273,
2.33519825400134));
#42980=CARTESIAN_POINT('Ctrl Pts',(-80.8554678524026,-4.03719872678699,
0.908392514475943));
#42981=CARTESIAN_POINT('Ctrl Pts',(-80.8090722417893,-4.07073536104181,
0.117473295968627));
#42982=CARTESIAN_POINT('Ctrl Pts',(-80.8021873309261,-4.07061909410162,
9.44285938865412E-5));
#42983=CARTESIAN_POINT('Origin',(-92.3478126690739,0.,0.));
#42984=CARTESIAN_POINT('',(-84.0978126690739,-4.07054770473266,0.000101237284119069));
#42985=CARTESIAN_POINT('',(-83.8021873309262,-4.07069555842019,-8.11031842548604E-5));
#42986=CARTESIAN_POINT('',(-92.3478126690739,-4.0705,-4.39132641279065E-13));
#42987=CARTESIAN_POINT('Ctrl Pts',(-84.0978126690739,-4.07054770473266,
0.000101237284118993));
#42988=CARTESIAN_POINT('Ctrl Pts',(-84.0665388911312,-4.07000484049112,
-0.533103383895171));
#42989=CARTESIAN_POINT('Ctrl Pts',(-83.9957544134385,-3.83156152900343,
-1.74041987047235));
#42990=CARTESIAN_POINT('Ctrl Pts',(-83.8854592359959,-2.67132578982276,
-3.29467473390518));
#42991=CARTESIAN_POINT('Ctrl Pts',(-83.7669271367457,-0.779329768066677,
-4.16935344990209));
#42992=CARTESIAN_POINT('Ctrl Pts',(-83.6483950374957,1.3008708565925,-4.03715222552651));
#42993=CARTESIAN_POINT('Ctrl Pts',(-83.5298629382456,3.06691707187941,-2.92999705662308));
#42994=CARTESIAN_POINT('Ctrl Pts',(-83.4113308389955,4.0923167299564,-1.11526089294132));
#42995=CARTESIAN_POINT('Ctrl Pts',(-83.2927987397454,4.12944046598591,0.968805716066663));
#42996=CARTESIAN_POINT('Ctrl Pts',(-83.1742666404953,3.16932306615985,2.81891014044657));
#42997=CARTESIAN_POINT('Ctrl Pts',(-83.0557345412452,1.44382852615606,3.98826055626553));
#42998=CARTESIAN_POINT('Ctrl Pts',(-82.9372024419952,-0.630344051771873,
4.19446414384497));
#42999=CARTESIAN_POINT('Ctrl Pts',(-82.818670342745,-2.55229140128288,3.38772367240052));
#43000=CARTESIAN_POINT('Ctrl Pts',(-82.7055404184379,-3.79836930332596,
1.83691733808824));
#43001=CARTESIAN_POINT('Ctrl Pts',(-82.6319211938809,-4.07016704624553,
0.581394268202383));
#43002=CARTESIAN_POINT('Ctrl Pts',(-82.5978126690739,-4.07069297892822,
-8.16732152923022E-5));
#43003=CARTESIAN_POINT('Ctrl Pts',(-83.8021873309262,-4.07069555842019,
-8.11031842551206E-5));
#43004=CARTESIAN_POINT('Ctrl Pts',(-83.7968397355401,-4.07077761748435,
-0.0912457722533375));
#43005=CARTESIAN_POINT('Ctrl Pts',(-83.751981440404,-4.04560590414255,-0.855935203987643));
#43006=CARTESIAN_POINT('Ctrl Pts',(-83.6676124455178,-3.58531215974383,
-2.26636268917237));
#43007=CARTESIAN_POINT('Ctrl Pts',(-83.5490803462679,-2.07279741151507,
-3.70059103556392));
#43008=CARTESIAN_POINT('Ctrl Pts',(-83.4305482470176,-0.0597114933943472,
-4.24114343771067));
#43009=CARTESIAN_POINT('Ctrl Pts',(-83.3120161477677,1.96779447944969,-3.75747894316481));
#43010=CARTESIAN_POINT('Ctrl Pts',(-83.1934840485175,3.52008701406145,-2.36640033280838));
#43011=CARTESIAN_POINT('Ctrl Pts',(-83.0749519492674,4.22229450661292,-0.403846779244268));
#43012=CARTESIAN_POINT('Ctrl Pts',(-82.9564198500173,3.90483703380788,1.65623393911674));
#43013=CARTESIAN_POINT('Ctrl Pts',(-82.8378877507673,2.64437913491587,3.31634167607942));
#43014=CARTESIAN_POINT('Ctrl Pts',(-82.7193556515171,0.745315673391867,
4.17556794564238));
#43015=CARTESIAN_POINT('Ctrl Pts',(-82.6008235522671,-1.33373814150481,
4.02641350230884));
#43016=CARTESIAN_POINT('Ctrl Pts',(-82.482291453017,-3.09070024685299,2.90489846737928));
#43017=CARTESIAN_POINT('Ctrl Pts',(-82.3827460459034,-3.93939696035747,
1.37388074382986));
#43018=CARTESIAN_POINT('Ctrl Pts',(-82.3227113385397,-4.07012516230206,
0.350009002499383));
#43019=CARTESIAN_POINT('Ctrl Pts',(-82.3021873309261,-4.07016134870022,
-1.1973211870471E-5));
#43020=CARTESIAN_POINT('Origin',(-92.3478126690739,0.,0.));
#43021=CARTESIAN_POINT('',(-85.5978126690739,-4.07017509531035,-3.25600794716127E-5));
#43022=CARTESIAN_POINT('',(-85.3021873309261,-4.07054479772079,0.000101412767817208));
#43023=CARTESIAN_POINT('',(-92.3478126690739,-4.0705,-4.39132641279065E-13));
#43024=CARTESIAN_POINT('Ctrl Pts',(-85.5978126690739,-4.07017509531035,
-3.25600794716038E-5));
#43025=CARTESIAN_POINT('Ctrl Pts',(-85.5801779878816,-4.07026000090821,
-0.300775414177721));
#43026=CARTESIAN_POINT('Ctrl Pts',(-85.5230326069393,-3.96366872821567,
-1.27527671801632));
#43027=CARTESIAN_POINT('Ctrl Pts',(-85.426376526247,-3.19411212591926,-2.79079035483874));
#43028=CARTESIAN_POINT('Ctrl Pts',(-85.3078444269969,-1.47901940386148,
-3.97534459897585));
#43029=CARTESIAN_POINT('Ctrl Pts',(-85.1893123277468,0.593249793413271,
-4.19987115995485));
#43030=CARTESIAN_POINT('Ctrl Pts',(-85.0707802284967,2.52225185735541,-3.41014789205285));
#43031=CARTESIAN_POINT('Ctrl Pts',(-84.9522481292466,3.84214154206329,-1.79688938122436));
#43032=CARTESIAN_POINT('Ctrl Pts',(-84.8337160299966,4.23417147746969,0.250309762069736));
#43033=CARTESIAN_POINT('Ctrl Pts',(-84.7151839307464,3.60366821294754,2.23706023356476));
#43034=CARTESIAN_POINT('Ctrl Pts',(-84.5966518314964,2.10289542607052,3.6835708089593));
#43035=CARTESIAN_POINT('Ctrl Pts',(-84.4781197322463,0.094282935351365,
4.24051574760746));
#43036=CARTESIAN_POINT('Ctrl Pts',(-84.3595876329963,-1.9370984564613,3.77339537387491));
#43037=CARTESIAN_POINT('Ctrl Pts',(-84.241055533746,-3.50067936031506,2.39501713853357));
#43038=CARTESIAN_POINT('Ctrl Pts',(-84.1537972124387,-4.02937512391122,
0.954530185624109));
#43039=CARTESIAN_POINT('Ctrl Pts',(-84.1060495908813,-4.07069068490978,
0.140537253042811));
#43040=CARTESIAN_POINT('Ctrl Pts',(-84.0978126690739,-4.07054770473266,
0.000101237284118993));
#43041=CARTESIAN_POINT('Ctrl Pts',(-85.3021873309262,-4.07054479772079,
0.000101412767817364));
#43042=CARTESIAN_POINT('Ctrl Pts',(-85.2709681325404,-4.07000279076567,
-0.53217374801187));
#43043=CARTESIAN_POINT('Ctrl Pts',(-85.2002382344046,-3.83218071396426,
-1.73856103852625));
#43044=CARTESIAN_POINT('Ctrl Pts',(-85.089997636519,-2.67358487308622,-3.29284178910621));
#43045=CARTESIAN_POINT('Ctrl Pts',(-84.9714655372688,-0.782189207191325,
-4.16881795786684));
#43046=CARTESIAN_POINT('Ctrl Pts',(-84.8529334380188,1.29810160318103,-4.03804350515179));
#43047=CARTESIAN_POINT('Ctrl Pts',(-84.7344013387685,3.06490676631494,-2.93209986792342));
#43048=CARTESIAN_POINT('Ctrl Pts',(-84.6158692395186,4.09155085191131,-1.11806741652885));
#43049=CARTESIAN_POINT('Ctrl Pts',(-84.4973371402684,4.13010397153302,0.965973242904165));
#43050=CARTESIAN_POINT('Ctrl Pts',(-84.3788050410185,3.17125572172011,2.81673574712594));
#43051=CARTESIAN_POINT('Ctrl Pts',(-84.2602729417682,1.44656360418077,3.98726934890774));
#43052=CARTESIAN_POINT('Ctrl Pts',(-84.1417408425183,-0.627467060215684,
4.19489549452951));
#43053=CARTESIAN_POINT('Ctrl Pts',(-84.0232087432681,-2.54996727660215,
3.38947341189422));
#43054=CARTESIAN_POINT('Ctrl Pts',(-83.9100242394041,-3.79771021737389,
1.83877430965476));
#43055=CARTESIAN_POINT('Ctrl Pts',(-83.8363504352901,-4.07017132422319,
0.582324235826637));
#43056=CARTESIAN_POINT('Ctrl Pts',(-83.8021873309262,-4.07069555842019,
-8.11031842551206E-5));
#43057=CARTESIAN_POINT('Origin',(-92.3478126690739,0.,0.));
#43058=CARTESIAN_POINT('',(-87.0978126690739,-4.07075463294496,-6.48897006623938E-5));
#43059=CARTESIAN_POINT('',(-86.8021873309262,-4.0701759211548,-3.33690431755795E-5));
#43060=CARTESIAN_POINT('',(-92.3478126690739,-4.0705,-4.39132641279065E-13));
#43061=CARTESIAN_POINT('Ctrl Pts',(-87.0978126690739,-4.07075463294496,
-6.48897006625716E-5));
#43062=CARTESIAN_POINT('Ctrl Pts',(-87.093817084632,-4.07080662684575,-0.0681779009651227));
#43063=CARTESIAN_POINT('Ctrl Pts',(-87.05031080044,-4.05257240534199,-0.809804772914534));
#43064=CARTESIAN_POINT('Ctrl Pts',(-86.9672938164981,-3.62329806373565,
-2.2051245358312));
#43065=CARTESIAN_POINT('Ctrl Pts',(-86.848761717248,-2.1353677918245,-3.66484208003093));
#43066=CARTESIAN_POINT('Ctrl Pts',(-86.730229617998,-0.131755887070526,
-4.23951689036003));
#43067=CARTESIAN_POINT('Ctrl Pts',(-86.6116975187478,1.90367446658495,-3.7903676078918));
#43068=CARTESIAN_POINT('Ctrl Pts',(-86.4931654194978,3.47937607418291,-2.42586174626368));
#43069=CARTESIAN_POINT('Ctrl Pts',(-86.3746333202476,4.21482414698068,-0.475521279897397));
#43070=CARTESIAN_POINT('Ctrl Pts',(-86.2561012209977,3.93241131237811,1.58965541797289));
#43071=CARTESIAN_POINT('Ctrl Pts',(-86.1375691217474,2.70033898852751,3.27093754520615));
#43072=CARTESIAN_POINT('Ctrl Pts',(-86.0190370224974,0.816147051306786,
4.16230309663427));
#43073=CARTESIAN_POINT('Ctrl Pts',(-85.9005049232474,-1.26514069566702,
4.04849133601287));
#43074=CARTESIAN_POINT('Ctrl Pts',(-85.7819728239972,-3.04090270501211,
2.95698728713125));
#43075=CARTESIAN_POINT('Ctrl Pts',(-85.6810754059395,-3.92736595192102,
1.42001385856659));
#43076=CARTESIAN_POINT('Ctrl Pts',(-85.6196886876317,-4.07006976896994,
0.373042302212225));
#43077=CARTESIAN_POINT('Ctrl Pts',(-85.5978126690739,-4.07017509531035,
-3.25600794716038E-5));
#43078=CARTESIAN_POINT('Ctrl Pts',(-86.8021873309262,-4.0701759211548,-3.33690431757877E-5));
#43079=CARTESIAN_POINT('Ctrl Pts',(-86.7846072292908,-4.07026268870466,
-0.299845247585942));
#43080=CARTESIAN_POINT('Ctrl Pts',(-86.7275164279055,-3.96410850627354,
-1.27341394546106));
#43081=CARTESIAN_POINT('Ctrl Pts',(-86.63091492677,-3.19602548924936,-2.78859896610174));
#43082=CARTESIAN_POINT('Ctrl Pts',(-86.51238282752,-1.48174561502481,-3.97432925838274));
#43083=CARTESIAN_POINT('Ctrl Pts',(-86.3938507282698,0.590369102043211,
-4.20027706765055));
#43084=CARTESIAN_POINT('Ctrl Pts',(-86.2753186290198,2.51991235967365,-3.41187702317127));
#43085=CARTESIAN_POINT('Ctrl Pts',(-86.1567865297697,3.84090821614495,-1.79952415844573));
#43086=CARTESIAN_POINT('Ctrl Pts',(-86.0382544305196,4.234342165928,0.247405625489327));
#43087=CARTESIAN_POINT('Ctrl Pts',(-85.9197223312695,3.6052016952943,2.23458807343251));
#43088=CARTESIAN_POINT('Ctrl Pts',(-85.8011902320195,2.10542137327692,3.68212764073006));
#43089=CARTESIAN_POINT('Ctrl Pts',(-85.6826581327693,0.0971913426281407,
4.24045008986049));
#43090=CARTESIAN_POINT('Ctrl Pts',(-85.5641260335193,-1.93450995627506,
3.77472308265816));
#43091=CARTESIAN_POINT('Ctrl Pts',(-85.4455939342692,-3.49903587826941,
2.39741757820016));
#43092=CARTESIAN_POINT('Ctrl Pts',(-85.3582810334048,-4.0290508143939,0.956392788326129));
#43093=CARTESIAN_POINT('Ctrl Pts',(-85.3104788322905,-4.07068874925191,
0.141468278350529));
#43094=CARTESIAN_POINT('Ctrl Pts',(-85.3021873309262,-4.07054479772079,
0.000101412767817364));
#43095=CARTESIAN_POINT('Origin',(-92.3478126690739,0.,0.));
#43096=CARTESIAN_POINT('',(-88.5978126690739,-4.07047297420895,0.00010377974335732));
#43097=CARTESIAN_POINT('',(-88.3021873309261,-4.07075680315938,-6.41537658660485E-5));
#43098=CARTESIAN_POINT('',(-92.3478126690739,-4.0705,-4.39132641279065E-13));
#43099=CARTESIAN_POINT('Ctrl Pts',(-88.5978126690739,-4.07047297420895,
0.000103779743357239));
#43100=CARTESIAN_POINT('Ctrl Pts',(-88.5679454816323,-4.0699633629615,-0.509146035156339));
#43101=CARTESIAN_POINT('Ctrl Pts',(-88.4985675944407,-3.84728083634177,
-1.69250630808891));
#43102=CARTESIAN_POINT('Ctrl Pts',(-88.3896790074992,-2.72914125118652,
-3.24694449006369));
#43103=CARTESIAN_POINT('Ctrl Pts',(-88.271146908249,-0.852900597114338,
-4.15492782628333));
#43104=CARTESIAN_POINT('Ctrl Pts',(-88.152614808999,1.22931172268961,-4.05951413513238));
#43105=CARTESIAN_POINT('Ctrl Pts',(-88.0340827097489,3.01465081869963,-2.98374660176146));
#43106=CARTESIAN_POINT('Ctrl Pts',(-87.9155506104989,4.07196543070694,-1.18741760272948));
#43107=CARTESIAN_POINT('Ctrl Pts',(-87.7970185112487,4.1459188620231,0.895667260529816));
#43108=CARTESIAN_POINT('Ctrl Pts',(-87.6784864119986,3.21865170212703,2.76245259353163));
#43109=CARTESIAN_POINT('Ctrl Pts',(-87.5599543127485,1.51409475903765,3.96211813494982));
#43110=CARTESIAN_POINT('Ctrl Pts',(-87.4414222134985,-0.556109197774073,
4.20495013639211));
#43111=CARTESIAN_POINT('Ctrl Pts',(-87.3228901142483,-2.49201530688875,
3.43230575316451));
#43112=CARTESIAN_POINT('Ctrl Pts',(-87.2083535994403,-3.78114015235693,
1.88476091323141));
#43113=CARTESIAN_POINT('Ctrl Pts',(-87.133327784382,-4.07029248043415,0.605363798947223));
#43114=CARTESIAN_POINT('Ctrl Pts',(-87.0978126690739,-4.07075463294496,
-6.48897006625716E-5));
#43115=CARTESIAN_POINT('Ctrl Pts',(-88.3021873309261,-4.07075680315937,
-6.4153765865849E-5));
#43116=CARTESIAN_POINT('Ctrl Pts',(-88.2982463260412,-4.07080763529163,
-0.0672466394881131));
#43117=CARTESIAN_POINT('Ctrl Pts',(-88.2547946214061,-4.05284527665673,
-0.807942598938564));
#43118=CARTESIAN_POINT('Ctrl Pts',(-88.1718322170211,-3.62480963907511,
-2.20263892537862));
#43119=CARTESIAN_POINT('Ctrl Pts',(-88.0533001177711,-2.13788088541058,
-3.6633766416475));
#43120=CARTESIAN_POINT('Ctrl Pts',(-87.9347680185209,-0.134663600797729,
-4.23942553278804));
#43121=CARTESIAN_POINT('Ctrl Pts',(-87.8162359192709,1.9010743336757,-3.79167238760187));
#43122=CARTESIAN_POINT('Ctrl Pts',(-87.6977038200208,3.47771144175241,-2.42824756783923));
#43123=CARTESIAN_POINT('Ctrl Pts',(-87.5791717207707,4.2144970165252,-0.478411976782104));
#43124=CARTESIAN_POINT('Ctrl Pts',(-87.4606396215207,3.93350068426081,1.58695793523026));
#43125=CARTESIAN_POINT('Ctrl Pts',(-87.3421075222705,2.70258178445977,3.26908470681113));
#43126=CARTESIAN_POINT('Ctrl Pts',(-87.2235754230204,0.819001646208479,
4.16174235447228));
#43127=CARTESIAN_POINT('Ctrl Pts',(-87.1050433237704,-1.2623636734931,4.04935810686113));
#43128=CARTESIAN_POINT('Ctrl Pts',(-86.9865112245203,-3.03887389383025,
2.95907224971836));
#43129=CARTESIAN_POINT('Ctrl Pts',(-86.8855592269055,-3.92687118700315,
1.42187609361087));
#43130=CARTESIAN_POINT('Ctrl Pts',(-86.8241179290408,-4.07006768149243,
0.373972080681628));
#43131=CARTESIAN_POINT('Ctrl Pts',(-86.8021873309262,-4.0701759211548,-3.33690431757877E-5));
#43132=CARTESIAN_POINT('Origin',(-59.25,4.52129938221115E-16,0.));
#43133=CARTESIAN_POINT('Ctrl Pts',(-59.25,3.73370339826923,1.62162243917753));
#43134=CARTESIAN_POINT('Ctrl Pts',(-59.25,3.70030638409769,1.72678322255912));
#43135=CARTESIAN_POINT('Ctrl Pts',(-59.25,3.66264502024489,1.83042819249524));
#43136=CARTESIAN_POINT('Ctrl Pts',(-59.25,3.62080294009585,1.93228746156618));
#43137=CARTESIAN_POINT('Ctrl Pts',(-59.25,3.57306535757599,2.04849858790993));
#43138=CARTESIAN_POINT('Ctrl Pts',(-59.25,3.51988717582558,2.16238619955646));
#43139=CARTESIAN_POINT('Ctrl Pts',(-59.25,3.46157351130409,2.27367045215858));
#43140=CARTESIAN_POINT('Ctrl Pts',(-59.25,3.42831099083415,2.33714776507546));
#43141=CARTESIAN_POINT('Ctrl Pts',(-59.25,3.3933765912802,2.39977793900337));
#43142=CARTESIAN_POINT('Ctrl Pts',(-59.25,3.35681960546461,2.46150741409173));
#43143=CARTESIAN_POINT('Ctrl Pts',(-59.25,3.33178364519508,2.50378269065766));
#43144=CARTESIAN_POINT('Ctrl Pts',(-59.25,3.30598655682051,2.54563549772312));
#43145=CARTESIAN_POINT('Ctrl Pts',(-59.25,3.27944283224882,2.58704812709493));
#43146=CARTESIAN_POINT('Ctrl Pts',(-59.25,3.26794189314794,2.60499150678627));
#43147=CARTESIAN_POINT('Ctrl Pts',(-59.25,3.25630353761244,2.62284785295622));
#43148=CARTESIAN_POINT('Ctrl Pts',(-59.25,3.24453365056515,2.64060915444784));
#43149=CARTESIAN_POINT('Ctrl Pts',(-59.25,3.17311768024368,2.74837914196769));
#43150=CARTESIAN_POINT('Ctrl Pts',(-59.25,3.09681512798329,2.85272629165589));
#43151=CARTESIAN_POINT('Ctrl Pts',(-59.25,3.01594945594691,2.95335783811544));
#43152=CARTESIAN_POINT('Ctrl Pts',(-59.25,2.93456493547749,3.05463505434908));
#43153=CARTESIAN_POINT('Ctrl Pts',(-59.25,2.84855818714407,3.15214957100135));
#43154=CARTESIAN_POINT('Ctrl Pts',(-59.25,2.7582089599964,3.24558571221565));
#43155=CARTESIAN_POINT('Ctrl Pts',(-59.25,2.72369285823248,3.28128110729978));
#43156=CARTESIAN_POINT('Ctrl Pts',(-59.25,2.68854249786815,3.31638103986582));
#43157=CARTESIAN_POINT('Ctrl Pts',(-59.25,2.65277174372166,3.35086689904567));
#43158=CARTESIAN_POINT('Ctrl Pts',(-59.25,2.63289346302342,3.37003114663433));
#43159=CARTESIAN_POINT('Ctrl Pts',(-59.25,2.61282357777559,3.38900574658438));
#43160=CARTESIAN_POINT('Ctrl Pts',(-59.25,2.59256434889638,3.40778741403533));
#43161=CARTESIAN_POINT('Ctrl Pts',(-59.25,2.57182031456538,3.4270185287396));
#43162=CARTESIAN_POINT('Ctrl Pts',(-59.25,2.55087325423301,3.44605124301962));
#43163=CARTESIAN_POINT('Ctrl Pts',(-59.25,2.52975088546925,3.46485978106417));
#43164=CARTESIAN_POINT('Ctrl Pts',(-59.25,2.47960903746643,3.50950888582762));
#43165=CARTESIAN_POINT('Ctrl Pts',(-59.25,2.42845837805422,3.5529152668294));
#43166=CARTESIAN_POINT('Ctrl Pts',(-59.25,2.37634253095915,3.59504099741696));
#43167=CARTESIAN_POINT('Ctrl Pts',(-59.25,2.27551221171727,3.67654309515114));
#43168=CARTESIAN_POINT('Ctrl Pts',(-59.25,2.17107182552093,3.75325338346143));
#43169=CARTESIAN_POINT('Ctrl Pts',(-59.25,2.06344354535521,3.82509569453245));
#43170=CARTESIAN_POINT('Ctrl Pts',(-59.25,1.95411483048912,3.89807305262374));
#43171=CARTESIAN_POINT('Ctrl Pts',(-59.25,1.84149617014203,3.96602787167803));
#43172=CARTESIAN_POINT('Ctrl Pts',(-59.25,1.72598702798438,4.02884810767464));
#43173=CARTESIAN_POINT('Ctrl Pts',(-59.25,1.6224562778767,4.08515383407155));
#43174=CARTESIAN_POINT('Ctrl Pts',(-59.25,1.51660255473828,4.13733445853516));
#43175=CARTESIAN_POINT('Ctrl Pts',(-59.25,1.40869034106602,4.18528315122508));
#43176=CARTESIAN_POINT('Ctrl Pts',(-59.25,1.32775618081182,4.22124467074251));
#43177=CARTESIAN_POINT('Ctrl Pts',(-59.25,1.24566363779897,4.25482524316704));
#43178=CARTESIAN_POINT('Ctrl Pts',(-59.25,1.1625182592197,4.2859693893738));
#43179=CARTESIAN_POINT('Ctrl Pts',(-59.25,1.14549561314186,4.29234564007268));
#43180=CARTESIAN_POINT('Ctrl Pts',(-59.25,1.12842677920724,4.29862046901966));
#43181=CARTESIAN_POINT('Ctrl Pts',(-59.25,1.11131922234629,4.30479098303606));
#43182=CARTESIAN_POINT('Ctrl Pts',(-59.25,0.98320067627071,4.35100198152908));
#43183=CARTESIAN_POINT('Ctrl Pts',(-59.25,0.85324085305285,4.39124906607606));
#43184=CARTESIAN_POINT('Ctrl Pts',(-59.25,0.721878465181344,4.42543828020427));
#43185=CARTESIAN_POINT('Ctrl Pts',(-59.25,0.613754215266846,4.4535793881171));
#43186=CARTESIAN_POINT('Ctrl Pts',(-59.25,0.504678753627349,4.47761582662026));
#43187=CARTESIAN_POINT('Ctrl Pts',(-59.25,0.39487946495906,4.49747515579454));
#43188=CARTESIAN_POINT('Ctrl Pts',(-59.25,0.262138836200427,4.52148387090821));
#43189=CARTESIAN_POINT('Ctrl Pts',(-59.25,0.128340414767412,4.53938931245444));
#43190=CARTESIAN_POINT('Ctrl Pts',(-59.25,-0.0061098054212493,4.55128614781597));
#43191=CARTESIAN_POINT('Ctrl Pts',(-59.25,-0.141656910697344,4.56328004111668));
#43192=CARTESIAN_POINT('Ctrl Pts',(-59.25,-0.27786725021061,4.56916700363061));
#43193=CARTESIAN_POINT('Ctrl Pts',(-59.25,-0.414338511577332,4.56899300375995));
#43194=CARTESIAN_POINT('Ctrl Pts',(-59.25,-0.46130902680036,4.56893311669294));
#43195=CARTESIAN_POINT('Ctrl Pts',(-59.25,-0.508310516274796,4.56815480456615));
#43196=CARTESIAN_POINT('Ctrl Pts',(-59.25,-0.555326693203861,4.56665852086362));
#43197=CARTESIAN_POINT('Ctrl Pts',(-59.25,-0.574417009651001,4.56605097403099));
#43198=CARTESIAN_POINT('Ctrl Pts',(-59.25,-0.593511702466989,4.56532496172441));
#43199=CARTESIAN_POINT('Ctrl Pts',(-59.25,-0.612603479656446,4.56448075813901));
#43200=CARTESIAN_POINT('Ctrl Pts',(-59.25,-0.751213987889701,4.55835165413454));
#43201=CARTESIAN_POINT('Ctrl Pts',(-59.25,-0.889274990910051,4.54601536277982));
#43202=CARTESIAN_POINT('Ctrl Pts',(-59.25,-1.02635580814156,4.52760979279899));
#43203=CARTESIAN_POINT('Ctrl Pts',(-59.25,-1.17093917736832,4.50819687001292));
#43204=CARTESIAN_POINT('Ctrl Pts',(-59.25,-1.31443290670101,4.48203265993226));
#43205=CARTESIAN_POINT('Ctrl Pts',(-59.25,-1.45634950900623,4.44921976842928));
#43206=CARTESIAN_POINT('Ctrl Pts',(-59.25,-1.59826611131146,4.41640687692631));
#43207=CARTESIAN_POINT('Ctrl Pts',(-59.25,-1.73860660530752,4.37694532748719));
#43208=CARTESIAN_POINT('Ctrl Pts',(-59.25,-1.87688689423306,4.33087666257546));
#43209=CARTESIAN_POINT('Ctrl Pts',(-59.25,-1.97170999958983,4.29928594273741));
#43210=CARTESIAN_POINT('Ctrl Pts',(-59.25,-2.06556440611198,4.26458709411248));
#43211=CARTESIAN_POINT('Ctrl Pts',(-59.25,-2.15833273047387,4.22686765274433));
#43212=CARTESIAN_POINT('Ctrl Pts',(-59.25,-2.19891887238219,4.21036539714576));
#43213=CARTESIAN_POINT('Ctrl Pts',(-59.25,-2.2392970843243,4.19328480879033));
#43214=CARTESIAN_POINT('Ctrl Pts',(-59.25,-2.27945727353288,4.17563243334272));
#43215=CARTESIAN_POINT('Ctrl Pts',(-59.25,-2.30456458384424,4.16459653742614));
#43216=CARTESIAN_POINT('Ctrl Pts',(-59.25,-2.32958667668184,4.15333714984871));
#43217=CARTESIAN_POINT('Ctrl Pts',(-59.25,-2.35452104605308,4.14185577889582));
#43218=CARTESIAN_POINT('Ctrl Pts',(-59.25,-2.37061736322258,4.13444400979725));
#43219=CARTESIAN_POINT('Ctrl Pts',(-59.25,-2.38667325540531,4.12694148008939));
#43220=CARTESIAN_POINT('Ctrl Pts',(-59.25,-2.40268097740313,4.11935218483388));
#43221=CARTESIAN_POINT('Ctrl Pts',(-59.25,-2.52978167954032,4.05909346995659));
#43222=CARTESIAN_POINT('Ctrl Pts',(-59.25,-2.65398157892713,3.99330674132034));
#43223=CARTESIAN_POINT('Ctrl Pts',(-59.25,-2.77498221207584,3.92231859342991));
#43224=CARTESIAN_POINT('Ctrl Pts',(-59.25,-2.89853629781064,3.84983239660291));
#43225=CARTESIAN_POINT('Ctrl Pts',(-59.25,-3.01875535833896,3.77192276608097));
#43226=CARTESIAN_POINT('Ctrl Pts',(-59.25,-3.13531440596932,3.68888383868272));
#43227=CARTESIAN_POINT('Ctrl Pts',(-59.25,-3.25228861614668,3.60554914142963));
#43228=CARTESIAN_POINT('Ctrl Pts',(-59.25,-3.36557741397246,3.51704820512911));
#43229=CARTESIAN_POINT('Ctrl Pts',(-59.25,-3.47483444492779,3.42362900180858));
#43230=CARTESIAN_POINT('Ctrl Pts',(-59.25,-3.58315056993114,3.33101431132959));
#43231=CARTESIAN_POINT('Ctrl Pts',(-59.25,-3.68750474245897,3.2335652796617));
#43232=CARTESIAN_POINT('Ctrl Pts',(-59.25,-3.78753162267819,3.13148094463183));
#43233=CARTESIAN_POINT('Ctrl Pts',(-59.25,-3.8168940019152,3.10151461005521));
#43234=CARTESIAN_POINT('Ctrl Pts',(-59.25,-3.84588328389748,3.07114859897418));
#43235=CARTESIAN_POINT('Ctrl Pts',(-59.25,-3.87448963569914,3.04038732119116));
#43236=CARTESIAN_POINT('',(-59.25,-4.77631074058413,-1.20178265305869));
#43237=CARTESIAN_POINT('Origin',(-59.25,0.,0.));
#43238=CARTESIAN_POINT('Ctrl Pts',(-59.25,-4.77631074058413,-1.20178265305869));
#43239=CARTESIAN_POINT('Ctrl Pts',(-59.25,-4.73353179200075,-1.32696589596601));
#43240=CARTESIAN_POINT('Ctrl Pts',(-59.25,-4.6857353234603,-1.45022519891399));
#43241=CARTESIAN_POINT('Ctrl Pts',(-59.25,-4.63294581112938,-1.57123974166275));
#43242=CARTESIAN_POINT('Ctrl Pts',(-59.25,-4.57511560091207,-1.70380956732513));
#43243=CARTESIAN_POINT('Ctrl Pts',(-59.25,-4.51129338536423,-1.83368642289548));
#43244=CARTESIAN_POINT('Ctrl Pts',(-59.25,-4.44173477384968,-1.96050991602634));
#43245=CARTESIAN_POINT('Ctrl Pts',(-59.25,-4.40262471266493,-2.03181775941211));
#43246=CARTESIAN_POINT('Ctrl Pts',(-59.25,-4.3617004223149,-2.10215974213619));
#43247=CARTESIAN_POINT('Ctrl Pts',(-59.25,-4.31900226670184,-2.17146662848551));
#43248=CARTESIAN_POINT('Ctrl Pts',(-59.25,-4.28594231940442,-2.22512894661517));
#43249=CARTESIAN_POINT('Ctrl Pts',(-59.25,-4.25181887239913,-2.27817065668745));
#43250=CARTESIAN_POINT('Ctrl Pts',(-59.25,-4.21664938444057,-2.33055784224177));
#43251=CARTESIAN_POINT('Ctrl Pts',(-59.25,-4.20538410111805,-2.34733819708897));
#43252=CARTESIAN_POINT('Ctrl Pts',(-59.25,-4.19401242684272,-2.36404991219832));
#43253=CARTESIAN_POINT('Ctrl Pts',(-59.25,-4.18254029751914,-2.3806843491385));
#43254=CARTESIAN_POINT('Ctrl Pts',(-59.25,-4.10178449304619,-2.4977792056528));
#43255=CARTESIAN_POINT('Ctrl Pts',(-59.25,-4.01598249499716,-2.61115479677391));
#43256=CARTESIAN_POINT('Ctrl Pts',(-59.25,-3.92538451237541,-2.72046840686664));
#43257=CARTESIAN_POINT('Ctrl Pts',(-59.25,-3.83550276971064,-2.82891781697254));
#43258=CARTESIAN_POINT('Ctrl Pts',(-59.25,-3.74089999144967,-2.93336972028254));
#43259=CARTESIAN_POINT('Ctrl Pts',(-59.25,-3.64178917502125,-3.03344935010836));
#43260=CARTESIAN_POINT('Ctrl Pts',(-59.25,-3.57026391056714,-3.10567377775125));
#43261=CARTESIAN_POINT('Ctrl Pts',(-59.25,-3.49639015724155,-3.17562028805039));
#43262=CARTESIAN_POINT('Ctrl Pts',(-59.25,-3.42024023020396,-3.24313265702998));
#43263=CARTESIAN_POINT('Ctrl Pts',(-59.25,-3.40538944723384,-3.25629894068275));
#43264=CARTESIAN_POINT('Ctrl Pts',(-59.25,-3.39045018710911,-3.26937423378017));
#43265=CARTESIAN_POINT('Ctrl Pts',(-59.25,-3.37542919856903,-3.28235193981733));
#43266=CARTESIAN_POINT('Ctrl Pts',(-59.25,-3.31342750193073,-3.33591963881594));
#43267=CARTESIAN_POINT('Ctrl Pts',(-59.25,-3.25009665988727,-3.38777142952235));
#43268=CARTESIAN_POINT('Ctrl Pts',(-59.25,-3.18548516409361,-3.43784341538071));
#43269=CARTESIAN_POINT('Ctrl Pts',(-59.25,-3.07590904070656,-3.52276164909831));
#43270=CARTESIAN_POINT('Ctrl Pts',(-59.25,-2.96265082171774,-3.60256350100977));
#43271=CARTESIAN_POINT('Ctrl Pts',(-59.25,-2.84610495743846,-3.67709913006717));
#43272=CARTESIAN_POINT('Ctrl Pts',(-59.25,-2.72927364023283,-3.75181731741237));
#43273=CARTESIAN_POINT('Ctrl Pts',(-59.25,-2.60913776602312,-3.8212437224481));
#43274=CARTESIAN_POINT('Ctrl Pts',(-59.25,-2.48607529075415,-3.88517902227304));
#43275=CARTESIAN_POINT('Ctrl Pts',(-59.25,-2.3787050182169,-3.94096166886738));
#43276=CARTESIAN_POINT('Ctrl Pts',(-59.25,-2.26910631512645,-3.99256368168234));
#43277=CARTESIAN_POINT('Ctrl Pts',(-59.25,-2.15752519659779,-4.03982030716511));
#43278=CARTESIAN_POINT('Ctrl Pts',(-59.25,-2.0738393577013,-4.07526277627718));
#43279=CARTESIAN_POINT('Ctrl Pts',(-59.25,-1.98903828425897,-4.10826035675606));
#43280=CARTESIAN_POINT('Ctrl Pts',(-59.25,-1.90322614380203,-4.13873171989141));
#43281=CARTESIAN_POINT('Ctrl Pts',(-59.25,-1.8843717581363,-4.14542679624371));
#43282=CARTESIAN_POINT('Ctrl Pts',(-59.25,-1.86546856747819,-4.1519998780532));
#43283=CARTESIAN_POINT('Ctrl Pts',(-59.25,-1.8465176865997,-4.15845003453348));
#43284=CARTESIAN_POINT('Ctrl Pts',(-59.25,-1.83130602442166,-4.16362750369719));
#43285=CARTESIAN_POINT('Ctrl Pts',(-59.25,-1.81606476693151,-4.16872534849972));
#43286=CARTESIAN_POINT('Ctrl Pts',(-59.25,-1.80080388427029,-4.17374013987465));
#43287=CARTESIAN_POINT('Ctrl Pts',(-59.25,-1.67249942992059,-4.21590153285044));
#43288=CARTESIAN_POINT('Ctrl Pts',(-59.25,-1.5426287282479,-4.25225822040849));
#43289=CARTESIAN_POINT('Ctrl Pts',(-59.25,-1.41154865683054,-4.28264911633847));
#43290=CARTESIAN_POINT('Ctrl Pts',(-59.25,-1.3124362801824,-4.30562830677922));
#43291=CARTESIAN_POINT('Ctrl Pts',(-59.25,-1.21263206758244,-4.32519576401433));
#43292=CARTESIAN_POINT('Ctrl Pts',(-59.25,-1.11228793538546,-4.34126217629354));
#43293=CARTESIAN_POINT('Ctrl Pts',(-59.25,-0.979035358188069,-4.36259766244154));
#43294=CARTESIAN_POINT('Ctrl Pts',(-59.25,-0.844829892568941,-4.37776087849656));
#43295=CARTESIAN_POINT('Ctrl Pts',(-59.25,-0.710100950691535,-4.38675752439951));
#43296=CARTESIAN_POINT('Ctrl Pts',(-59.25,-0.576496800019825,-4.39567906136112));
#43297=CARTESIAN_POINT('Ctrl Pts',(-59.25,-0.442377092384796,-4.3985363451751));
#43298=CARTESIAN_POINT('Ctrl Pts',(-59.25,-0.308176480047048,-4.39528647850796));
#43299=CARTESIAN_POINT('Ctrl Pts',(-59.25,-0.261458280238702,-4.39415512807922));
#43300=CARTESIAN_POINT('Ctrl Pts',(-59.25,-0.214730472181454,-4.39228324020791));
#43301=CARTESIAN_POINT('Ctrl Pts',(-59.25,-0.168012117042926,-4.38966768275966));
#43302=CARTESIAN_POINT('Ctrl Pts',(-59.25,-0.142145356406747,-4.38821951536928));
#43303=CARTESIAN_POINT('Ctrl Pts',(-59.25,-0.116275424988109,-4.38654282160773));
#43304=CARTESIAN_POINT('Ctrl Pts',(-59.25,-0.0904392486155291,-4.38463973183507));
#43305=CARTESIAN_POINT('Ctrl Pts',(-59.25,0.0410133206382076,-4.37495695074047));
#43306=CARTESIAN_POINT('Ctrl Pts',(-59.25,0.171725828963868,-4.35941295456871));
#43307=CARTESIAN_POINT('Ctrl Pts',(-59.25,0.301301898250337,-4.33804997480716));
#43308=CARTESIAN_POINT('Ctrl Pts',(-59.25,0.429447519281489,-4.31692283054592));
#43309=CARTESIAN_POINT('Ctrl Pts',(-59.25,0.556482392005791,-4.29010420308145));
#43310=CARTESIAN_POINT('Ctrl Pts',(-59.25,0.682008049033365,-4.25758697212456));
#43311=CARTESIAN_POINT('Ctrl Pts',(-59.25,0.802901216297604,-4.22626978061066));
#43312=CARTESIAN_POINT('Ctrl Pts',(-59.25,0.922395005914746,-4.18966643744355));
#43313=CARTESIAN_POINT('Ctrl Pts',(-59.25,1.04011060800678,-4.14773097044074));
#43314=CARTESIAN_POINT('Ctrl Pts',(-59.25,1.12177492014559,-4.11863855612911));
#43315=CARTESIAN_POINT('Ctrl Pts',(-59.25,1.2025829258255,-4.08697895456957));
#43316=CARTESIAN_POINT('Ctrl Pts',(-59.25,1.2824204934428,-4.05280356580097));
#43317=CARTESIAN_POINT('Ctrl Pts',(-59.25,1.32283749131235,-4.03550260515957));
#43318=CARTESIAN_POINT('Ctrl Pts',(-59.25,1.36300566803296,-4.01755679371646));
#43319=CARTESIAN_POINT('Ctrl Pts',(-59.25,1.40290943437871,-3.99897218974183));
#43320=CARTESIAN_POINT('Ctrl Pts',(-59.25,1.42483837727862,-3.98875910068537));
#43321=CARTESIAN_POINT('Ctrl Pts',(-59.25,1.44668745843242,-3.97835308915049));
#43322=CARTESIAN_POINT('Ctrl Pts',(-59.25,1.46845401683104,-3.96775511286795));
#43323=CARTESIAN_POINT('Ctrl Pts',(-59.25,1.48305813660077,-3.96064447497506));
#43324=CARTESIAN_POINT('Ctrl Pts',(-59.25,1.49762227703197,-3.95344876155404));
#43325=CARTESIAN_POINT('Ctrl Pts',(-59.25,1.51213804695255,-3.94617228279005));
#43326=CARTESIAN_POINT('Ctrl Pts',(-59.25,1.62935001463851,-3.88741615766419));
#43327=CARTESIAN_POINT('Ctrl Pts',(-59.25,1.74355939590811,-3.82332582185838));
#43328=CARTESIAN_POINT('Ctrl Pts',(-59.25,1.85442498273839,-3.75415630054696));
#43329=CARTESIAN_POINT('Ctrl Pts',(-59.25,1.96237767301167,-3.68680414805339));
#43330=CARTESIAN_POINT('Ctrl Pts',(-59.25,2.06716045912934,-3.61463545217675));
#43331=CARTESIAN_POINT('Ctrl Pts',(-59.25,2.16842427848398,-3.53784621807521));
#43332=CARTESIAN_POINT('Ctrl Pts',(-59.25,2.27378671312092,-3.45794896839208));
#43333=CARTESIAN_POINT('Ctrl Pts',(-59.25,2.37534057096294,-3.37304919561452));
#43334=CARTESIAN_POINT('Ctrl Pts',(-59.25,2.47264335148199,-3.2833325165496));
#43335=CARTESIAN_POINT('Ctrl Pts',(-59.25,2.56305105159527,-3.19997335072932));
#43336=CARTESIAN_POINT('Ctrl Pts',(-59.25,2.64978877207528,-3.11245500767447));
#43337=CARTESIAN_POINT('Ctrl Pts',(-59.25,2.73245446931944,-3.02090586202492));
#43338=CARTESIAN_POINT('Ctrl Pts',(-59.25,2.73875909413107,-3.01392372754366));
#43339=CARTESIAN_POINT('Ctrl Pts',(-59.25,2.74504000957142,-3.00691814002619));
#43340=CARTESIAN_POINT('Ctrl Pts',(-59.25,2.75129702511905,-2.99988915288066));
#43341=CARTESIAN_POINT('Ctrl Pts',(-90.0683458050225,-1.79217368492204,
3.6547344271606));
#43342=CARTESIAN_POINT('Ctrl Pts',(-90.0288351052725,-2.39703965939263,
3.35812604043492));
#43343=CARTESIAN_POINT('Ctrl Pts',(-89.9498137057724,-3.4560716865392,2.45910294398196));
#43344=CARTESIAN_POINT('Ctrl Pts',(-89.8312816065225,-4.21012624900965,
0.515537866574306));
#43345=CARTESIAN_POINT('Ctrl Pts',(-89.7127495072723,-3.94736126811263,
-1.55208240117109));
#43346=CARTESIAN_POINT('Ctrl Pts',(-89.5942174080221,-2.73137303949805,
-3.24509720256334));
#43347=CARTESIAN_POINT('Ctrl Pts',(-89.4756853087722,-0.855747416393033,
-4.15432931934335));
#43348=CARTESIAN_POINT('Ctrl Pts',(-89.357153209522,1.22652580399161,-4.06036256423134));
#43349=CARTESIAN_POINT('Ctrl Pts',(-89.2386211102719,3.0126043279509,-2.98581045744857));
#43350=CARTESIAN_POINT('Ctrl Pts',(-89.1200890110218,4.07114973607406,-1.19021168789138));
#43351=CARTESIAN_POINT('Ctrl Pts',(-89.0015569117718,4.14653236502477,0.892824265437017));
#43352=CARTESIAN_POINT('Ctrl Pts',(-88.8830248125217,3.22054554208703,2.76024400176603));
#43353=CARTESIAN_POINT('Ctrl Pts',(-88.7644927132716,1.51681193095975,3.96107892847728));
#43354=CARTESIAN_POINT('Ctrl Pts',(-88.6459606140215,-0.553225051728948,
4.20533047603355));
#43355=CARTESIAN_POINT('Ctrl Pts',(-88.5274285147713,-2.48966060894145,
3.43401418720049));
#43356=CARTESIAN_POINT('Ctrl Pts',(-88.4088964155214,-3.82485446805869,
1.83339885856207));
#43357=CARTESIAN_POINT('Ctrl Pts',(-88.2903643162712,-4.23636330669712,
-0.209973878906397));
#43358=CARTESIAN_POINT('Ctrl Pts',(-88.1718322170211,-3.62480963907511,
-2.20263892537862));
#43359=CARTESIAN_POINT('Ctrl Pts',(-88.0533001177711,-2.13788088541058,
-3.6633766416475));
#43360=CARTESIAN_POINT('Ctrl Pts',(-87.9347680185209,-0.134663600797729,
-4.23942553278804));
#43361=CARTESIAN_POINT('Ctrl Pts',(-87.8162359192709,1.9010743336757,-3.79167238760187));
#43362=CARTESIAN_POINT('Ctrl Pts',(-87.6977038200208,3.47771144175241,-2.42824756783923));
#43363=CARTESIAN_POINT('Ctrl Pts',(-87.5791717207707,4.2144970165252,-0.478411976782104));
#43364=CARTESIAN_POINT('Ctrl Pts',(-87.4606396215207,3.93350068426081,1.58695793523026));
#43365=CARTESIAN_POINT('Ctrl Pts',(-87.3421075222705,2.70258178445977,3.26908470681113));
#43366=CARTESIAN_POINT('Ctrl Pts',(-87.2235754230204,0.819001646208479,
4.16174235447228));
#43367=CARTESIAN_POINT('Ctrl Pts',(-87.1050433237704,-1.2623636734931,4.04935810686113));
#43368=CARTESIAN_POINT('Ctrl Pts',(-86.9865112245203,-3.03887389383025,
2.95907224971836));
#43369=CARTESIAN_POINT('Ctrl Pts',(-86.8679791252702,-4.08150985721014,
1.15418387061051));
#43370=CARTESIAN_POINT('Ctrl Pts',(-86.7494470260202,-4.13847970927864,
-0.929434676334609));
#43371=CARTESIAN_POINT('Ctrl Pts',(-86.63091492677,-3.19602548924936,-2.78859896610174));
#43372=CARTESIAN_POINT('Ctrl Pts',(-86.51238282752,-1.48174561502481,-3.97432925838274));
#43373=CARTESIAN_POINT('Ctrl Pts',(-86.3938507282698,0.590369102043211,
-4.20027706765055));
#43374=CARTESIAN_POINT('Ctrl Pts',(-86.2753186290198,2.51991235967365,-3.41187702317127));
#43375=CARTESIAN_POINT('Ctrl Pts',(-86.1567865297697,3.84090821614495,-1.79952415844573));
#43376=CARTESIAN_POINT('Ctrl Pts',(-86.0382544305196,4.234342165928,0.247405625489327));
#43377=CARTESIAN_POINT('Ctrl Pts',(-85.9197223312695,3.6052016952943,2.23458807343251));
#43378=CARTESIAN_POINT('Ctrl Pts',(-85.8011902320195,2.10542137327692,3.68212764073006));
#43379=CARTESIAN_POINT('Ctrl Pts',(-85.6826581327693,0.0971913426281407,
4.24045008986049));
#43380=CARTESIAN_POINT('Ctrl Pts',(-85.5641260335193,-1.93450995627506,
3.77472308265816));
#43381=CARTESIAN_POINT('Ctrl Pts',(-85.4455939342692,-3.49903587826941,
2.39741757820016));
#43382=CARTESIAN_POINT('Ctrl Pts',(-85.3270618350191,-4.21856051198106,
0.441146606508185));
#43383=CARTESIAN_POINT('Ctrl Pts',(-85.2085297357689,-3.91932192309739,
-1.62165926902288));
#43384=CARTESIAN_POINT('Ctrl Pts',(-85.089997636519,-2.67358487308622,-3.29284178910621));
#43385=CARTESIAN_POINT('Ctrl Pts',(-84.9714655372688,-0.782189207191325,
-4.16881795786684));
#43386=CARTESIAN_POINT('Ctrl Pts',(-84.8529334380188,1.29810160318103,-4.03804350515179));
#43387=CARTESIAN_POINT('Ctrl Pts',(-84.7344013387685,3.06490676631494,-2.93209986792342));
#43388=CARTESIAN_POINT('Ctrl Pts',(-84.6158692395186,4.09155085191131,-1.11806741652885));
#43389=CARTESIAN_POINT('Ctrl Pts',(-84.4973371402684,4.13010397153302,0.965973242904165));
#43390=CARTESIAN_POINT('Ctrl Pts',(-84.3788050410185,3.17125572172011,2.81673574712594));
#43391=CARTESIAN_POINT('Ctrl Pts',(-84.2602729417682,1.44656360418077,3.98726934890774));
#43392=CARTESIAN_POINT('Ctrl Pts',(-84.1417408425183,-0.627467060215684,
4.19489549452951));
#43393=CARTESIAN_POINT('Ctrl Pts',(-84.0232087432681,-2.54996727660215,
3.38947341189422));
#43394=CARTESIAN_POINT('Ctrl Pts',(-83.904676644018,-3.85666196576058,1.76550887948358));
#43395=CARTESIAN_POINT('Ctrl Pts',(-83.786144544768,-4.23199028917877,-0.284818036606317));
#43396=CARTESIAN_POINT('Ctrl Pts',(-83.6676124455178,-3.58531215974383,
-2.26636268917237));
#43397=CARTESIAN_POINT('Ctrl Pts',(-83.5490803462679,-2.07279741151507,
-3.70059103556392));
#43398=CARTESIAN_POINT('Ctrl Pts',(-83.4305482470176,-0.0597114933943472,
-4.24114343771067));
#43399=CARTESIAN_POINT('Ctrl Pts',(-83.3120161477677,1.96779447944969,-3.75747894316481));
#43400=CARTESIAN_POINT('Ctrl Pts',(-83.1934840485175,3.52008701406145,-2.36640033280838));
#43401=CARTESIAN_POINT('Ctrl Pts',(-83.0749519492674,4.22229450661292,-0.403846779244268));
#43402=CARTESIAN_POINT('Ctrl Pts',(-82.9564198500173,3.90483703380788,1.65623393911674));
#43403=CARTESIAN_POINT('Ctrl Pts',(-82.8378877507673,2.64437913491587,3.31634167607942));
#43404=CARTESIAN_POINT('Ctrl Pts',(-82.7193556515171,0.745315673391867,
4.17556794564238));
#43405=CARTESIAN_POINT('Ctrl Pts',(-82.6008235522671,-1.33373814150481,
4.02641350230884));
#43406=CARTESIAN_POINT('Ctrl Pts',(-82.482291453017,-3.09070024685299,2.90489846737928));
#43407=CARTESIAN_POINT('Ctrl Pts',(-82.363759353767,-4.1012722661475,1.0818636330929));
#43408=CARTESIAN_POINT('Ctrl Pts',(-82.2452272545168,-4.1214056420387,-1.00243635980107));
#43409=CARTESIAN_POINT('Ctrl Pts',(-82.1266951552668,-3.14623825560085,
-2.84465252019879));
#43410=CARTESIAN_POINT('Ctrl Pts',(-82.0081630560165,-1.41126860599162,
-3.99989800412737));
#43411=CARTESIAN_POINT('Ctrl Pts',(-81.8896309567667,0.664516008557521,
-4.18918626896089));
#43412=CARTESIAN_POINT('Ctrl Pts',(-81.7710988575164,2.57982302217583,-3.36680505760746));
#43413=CARTESIAN_POINT('Ctrl Pts',(-81.6525667582664,3.87211448147575,-1.73135570118489));
#43414=CARTESIAN_POINT('Ctrl Pts',(-81.5340346590163,4.22930786260355,0.322208201322427));
#43415=CARTESIAN_POINT('Ctrl Pts',(-81.4155025597663,3.56514258472508,2.29796028517889));
#43416=CARTESIAN_POINT('Ctrl Pts',(-81.2969704605161,2.04001154890355,3.71876538679436));
#43417=CARTESIAN_POINT('Ctrl Pts',(-81.178438361266,0.0222269802501248,
4.24150552080608));
#43418=CARTESIAN_POINT('Ctrl Pts',(-81.0599062620159,-2.00092530328236,
3.73994131670062));
#43419=CARTESIAN_POINT('Ctrl Pts',(-80.9413741627659,-3.54086320495273,
2.33519825400134));
#43420=CARTESIAN_POINT('Ctrl Pts',(-80.8228420635157,-4.22569870873143,
0.366515408552093));
#43421=CARTESIAN_POINT('Ctrl Pts',(-80.7043099642657,-3.8900471477876,-1.69067924505763));
#43422=CARTESIAN_POINT('Ctrl Pts',(-80.5857778650156,-2.61496685112479,
-3.33958253217321));
#43423=CARTESIAN_POINT('Ctrl Pts',(-80.4672457657655,-0.708383924910281,
-4.18199179059653));
#43424=CARTESIAN_POINT('Ctrl Pts',(-80.3487136665154,1.36927050498713,-4.01446900670923));
#43425=CARTESIAN_POINT('Ctrl Pts',(-80.2301815672654,3.11625232078442,-2.87747017272681));
#43426=CARTESIAN_POINT('Ctrl Pts',(-80.1116494680153,4.11067334059816,-1.04557534807476));
#43427=CARTESIAN_POINT('Ctrl Pts',(-79.9931173687652,4.11238540021266,1.03882117896535));
#43428=CARTESIAN_POINT('Ctrl Pts',(-79.8745852695151,3.12097504491475,2.87234710485192));
#43429=CARTESIAN_POINT('Ctrl Pts',(-79.756053170265,1.37586337731199,4.01221423757314));
#43430=CARTESIAN_POINT('Ctrl Pts',(-79.6375210710149,-0.701513053379031,
4.18314983703188));
#43431=CARTESIAN_POINT('Ctrl Pts',(-79.5189889717648,-2.60947726422201,
3.343873730567));
#43432=CARTESIAN_POINT('Ctrl Pts',(-79.4004568725148,-3.88726455677248,
1.69706729179175));
#43433=CARTESIAN_POINT('Ctrl Pts',(-79.2819247732647,-4.22629509483729,
-0.359573200448428));
#43434=CARTESIAN_POINT('Ctrl Pts',(-79.1633926740146,-3.54469454740893,
-2.32937839090772));
#43435=CARTESIAN_POINT('Ctrl Pts',(-79.0448605747645,-2.00706634268101,
-3.73664927998142));
#43436=CARTESIAN_POINT('Ctrl Pts',(-78.9263284755144,0.0152592617744791,
-4.24153630056935));
#43437=CARTESIAN_POINT('Ctrl Pts',(-78.8077963762643,2.03389985453592,-3.72211159382277));
#43438=CARTESIAN_POINT('Ctrl Pts',(-78.6892642770142,3.56136279891019,-2.30381373712066));
#43439=CARTESIAN_POINT('Ctrl Pts',(-78.5707321777641,4.22877291137641,-0.329155494427314));
#43440=CARTESIAN_POINT('Ctrl Pts',(-78.4522000785141,3.87495330153115,1.72499266588648));
#43441=CARTESIAN_POINT('Ctrl Pts',(-78.333667979264,2.58535055813011,3.36256220074308));
#43442=CARTESIAN_POINT('Ctrl Pts',(-78.2151358800139,0.671396364788188,
4.18808967855972));
#43443=CARTESIAN_POINT('Ctrl Pts',(-78.0966037807638,-1.40469494822981,
4.00220956636128));
#43444=CARTESIAN_POINT('Ctrl Pts',(-77.9780716815137,-3.14156294622147,
2.84981991591854));
#43445=CARTESIAN_POINT('Ctrl Pts',(-77.8595395822636,-4.11974940532679,
1.00919977696215));
#43446=CARTESIAN_POINT('Ctrl Pts',(-77.7410074830135,-4.10305187789505,
-1.07511354071959));
#43447=CARTESIAN_POINT('Ctrl Pts',(-77.6224753837634,-3.09545209551088,
-2.89984013449786));
#43448=CARTESIAN_POINT('Ctrl Pts',(-77.5039432845133,-1.34038284556851,
-4.02417116971747));
#43449=CARTESIAN_POINT('Ctrl Pts',(-77.3854111852633,0.738520086648723,
-4.17687915873197));
#43450=CARTESIAN_POINT('Ctrl Pts',(-77.2668790860131,2.63879720128349,-3.32049492888954));
#43451=CARTESIAN_POINT('Ctrl Pts',(-77.1483469867632,3.90237383473824,-1.66302156401962));
#43452=CARTESIAN_POINT('Ctrl Pts',(-77.0298148875129,4.22242284177216,0.397665888508434));
#43453=CARTESIAN_POINT('Ctrl Pts',(-76.911282788263,3.52503575024894,2.35909274883029));
#43454=CARTESIAN_POINT('Ctrl Pts',(-76.7927506890127,1.97181984252191,3.75729912712469));
#43455=CARTESIAN_POINT('Ctrl Pts',(-76.6742185897627,-0.0484579238967644,
4.23516823465935));
#43456=CARTESIAN_POINT('Ctrl Pts',(-76.5161757907627,-2.75000559908163,
3.54082966140385));
#43457=CARTESIAN_POINT('Ctrl Pts',(-76.3186222920125,-4.79203870408418,
0.336434116267563));
#43458=CARTESIAN_POINT('Ctrl Pts',(-76.0815580935123,-2.89441002508752,
-3.83698970964484));
#43459=CARTESIAN_POINT('Ctrl Pts',(-75.8444938950122,1.63095801340486,-4.51688897627564));
#43460=CARTESIAN_POINT('Ctrl Pts',(-75.607429696512,4.67567242759371,-1.10249052069397));
#43461=CARTESIAN_POINT('Ctrl Pts',(-75.3703654980118,3.47661902182452,3.31543652103366));
#43462=CARTESIAN_POINT('Ctrl Pts',(-75.1333012995117,-0.878131813745364,
4.72260507390595));
#43463=CARTESIAN_POINT('Ctrl Pts',(-74.8962371010114,-4.43574436453777,
1.84399067006013));
#43464=CARTESIAN_POINT('Ctrl Pts',(-74.6591729025114,-3.96732235451901,
-2.70870511280469));
#43465=CARTESIAN_POINT('Ctrl Pts',(-74.422108704011,0.102291553945791,-4.80267280759255));
#43466=CARTESIAN_POINT('Ctrl Pts',(-74.185044505511,4.07867853910156,-2.53741907084073));
#43467=CARTESIAN_POINT('Ctrl Pts',(-73.9479803070107,4.35373227228281,2.03076696083007));
#43468=CARTESIAN_POINT('Ctrl Pts',(-73.7109161085106,0.675669024164784,
4.75614017541162));
#43469=CARTESIAN_POINT('Ctrl Pts',(-73.4738519100105,-3.6129693088472,3.16366288324438));
#43470=CARTESIAN_POINT('Ctrl Pts',(-73.2367877115102,-4.62749258109677,
-1.29861920405548));
#43471=CARTESIAN_POINT('Ctrl Pts',(-72.9997235130101,-1.43150958571139,
-4.58558645780951));
#43472=CARTESIAN_POINT('Ctrl Pts',(-72.8021700142599,2.29645120176649,-3.85049572963833));
#43473=CARTESIAN_POINT('Ctrl Pts',(-72.6441272152598,3.92679810234926,-1.58721605638371));
#43474=CARTESIAN_POINT('Ctrl Pts',(-72.5255951160097,4.21734429791554,0.468377299721421));
#43475=CARTESIAN_POINT('Ctrl Pts',(-72.4070630167596,3.4806665638518,2.42407836288371));
#43476=CARTESIAN_POINT('Ctrl Pts',(-72.2885309175095,1.90781163232082,3.78777607431905));
#43477=CARTESIAN_POINT('Ctrl Pts',(-72.1699988182595,-0.127952933172336,
4.24002244278688));
#43478=CARTESIAN_POINT('Ctrl Pts',(-72.0514667190093,-2.13173404035006,
3.66669431825119));
#43479=CARTESIAN_POINT('Ctrl Pts',(-71.9329346197594,-3.62124894073959,
2.20868457101181));
#43480=CARTESIAN_POINT('Ctrl Pts',(-71.8144025205091,-4.23598160600254,
0.216886167119235));
#43481=CARTESIAN_POINT('Ctrl Pts',(-71.6958704212593,-3.82787651363011,
-1.82709000261242));
#43482=CARTESIAN_POINT('Ctrl Pts',(-71.5773383220089,-2.49529078987354,
-3.42993115267771));
#43483=CARTESIAN_POINT('Ctrl Pts',(-71.458806222759,-0.560136340693826,
-4.20441037867915));
#43484=CARTESIAN_POINT('Ctrl Pts',(-71.3402741235088,1.5103047169698,-3.96356795830934));
#43485=CARTESIAN_POINT('Ctrl Pts',(-71.2217420242588,3.21600598369556,-2.76552975458416));
#43486=CARTESIAN_POINT('Ctrl Pts',(-71.1032099250086,4.14506039630085,-0.899634673257719));
#43487=CARTESIAN_POINT('Ctrl Pts',(-70.9846778257586,4.07309954546553,1.18352108347017));
#43488=CARTESIAN_POINT('Ctrl Pts',(-70.8661457265085,3.01750462107274,2.98086038723955));
#43489=CARTESIAN_POINT('Ctrl Pts',(-70.7476136272584,1.23319553280523,4.0583361681078));
#43490=CARTESIAN_POINT('Ctrl Pts',(-70.6290815280083,-0.848924438267781,
4.15574181331312));
#43491=CARTESIAN_POINT('Ctrl Pts',(-70.5105494287582,-2.72603312996977,
3.24955484789199));
#43492=CARTESIAN_POINT('Ctrl Pts',(-70.3920173295082,-3.94481712984691,
1.5586150410489));
#43493=CARTESIAN_POINT('Ctrl Pts',(-70.273485230258,-4.21094572157516,-0.508723181559844));
#43494=CARTESIAN_POINT('Ctrl Pts',(-70.154953131008,-3.46015001328113,-2.45320708625443));
#43495=CARTESIAN_POINT('Ctrl Pts',(-70.0364210317579,-1.87374378398806,
-3.80525259964336));
#43496=CARTESIAN_POINT('Ctrl Pts',(-69.9178889325078,0.165163070961228,
-4.23834688141492));
#43497=CARTESIAN_POINT('Ctrl Pts',(-69.7993568332577,2.16418379186852,-3.64789961943599));
#43498=CARTESIAN_POINT('Ctrl Pts',(-69.6808247340076,3.64056394757633,-2.17650115247581));
#43499=CARTESIAN_POINT('Ctrl Pts',(-69.5622926347575,4.2377644279798,-0.179487532051847));
#43500=CARTESIAN_POINT('Ctrl Pts',(-69.4437605355075,3.81156402742994,1.8608715126343));
#43501=CARTESIAN_POINT('Ctrl Pts',(-69.3252284362573,2.46488820851225,3.45183853059299));
#43502=CARTESIAN_POINT('Ctrl Pts',(-69.2066963370073,0.522953071331976,
4.20920220550053));
#43503=CARTESIAN_POINT('Ctrl Pts',(-69.0881642377572,-1.54527285978556,
3.95006264640662));
#43504=CARTESIAN_POINT('Ctrl Pts',(-68.9696321385071,-3.24032240668157,
2.737000880967));
#43505=CARTESIAN_POINT('Ctrl Pts',(-68.851100039257,-4.15284879481873,0.862965821490488));
#43506=CARTESIAN_POINT('Ctrl Pts',(-68.7325679400069,-4.06248104189545,
-1.21947156831061));
#43507=CARTESIAN_POINT('Ctrl Pts',(-68.6140358407569,-2.99104255021837,
-3.00741210752073));
#43508=CARTESIAN_POINT('Ctrl Pts',(-68.4955037415068,-1.19728085404309,
-4.06907626842045));
#43509=CARTESIAN_POINT('Ctrl Pts',(-68.3769716422567,0.885618735911535,
-4.14807697328309));
#43510=CARTESIAN_POINT('Ctrl Pts',(-68.2584395430066,2.75464541949803,-3.22533591033841));
#43511=CARTESIAN_POINT('Ctrl Pts',(-68.1399074437565,3.9584377330416,-1.52369085949611));
#43512=CARTESIAN_POINT('Ctrl Pts',(-68.0213753445065,4.20628529483797,0.54591862040923));
#43513=CARTESIAN_POINT('Ctrl Pts',(-67.9028432452563,3.43833404328219,2.48369123050478));
#43514=CARTESIAN_POINT('Ctrl Pts',(-67.7843111460063,1.84004072116821,3.82166367778779));
#43515=CARTESIAN_POINT('Ctrl Pts',(-67.6657790467562,-0.202614086215485,
4.23672168707678));
#43516=CARTESIAN_POINT('Ctrl Pts',(-67.5472469475061,-2.19633851110734,
3.62863063238826));
#43517=CARTESIAN_POINT('Ctrl Pts',(-67.428714848256,-3.65965715110381,2.14424174431298));
#43518=CARTESIAN_POINT('Ctrl Pts',(-67.3101827490059,-4.23918519422161,
0.142028204142372));
#43519=CARTESIAN_POINT('Ctrl Pts',(-67.1916506497558,-3.79496924756422,
-1.89448450289823));
#43520=CARTESIAN_POINT('Ctrl Pts',(-67.0731185505057,-2.43428544669007,
-3.47348779841137));
#43521=CARTESIAN_POINT('Ctrl Pts',(-66.9545864512557,-0.485732755623718,
-4.21365955100716));
#43522=CARTESIAN_POINT('Ctrl Pts',(-66.8360543520056,1.58012219199054,-3.93625164084547));
#43523=CARTESIAN_POINT('Ctrl Pts',(-66.7175222527555,3.26438479979246,-2.70825681953606));
#43524=CARTESIAN_POINT('Ctrl Pts',(-66.5989901535054,4.16031329007191,-0.826230264593738));
#43525=CARTESIAN_POINT('Ctrl Pts',(-66.4804580542553,4.05154499755959,1.25532715035943));
#43526=CARTESIAN_POINT('Ctrl Pts',(-66.3619259550052,2.96434697137833,3.03372875434832));
#43527=CARTESIAN_POINT('Ctrl Pts',(-66.2433938557551,1.16127260186261,4.07949862922429));
#43528=CARTESIAN_POINT('Ctrl Pts',(-66.124861756505,-0.922243831912986,
4.14008809521949));
#43529=CARTESIAN_POINT('Ctrl Pts',(-66.006329657255,-2.78304256481646,3.20086507121113));
#43530=CARTESIAN_POINT('Ctrl Pts',(-65.8877975580049,-3.97174914593023,
1.48864765592202));
#43531=CARTESIAN_POINT('Ctrl Pts',(-65.7692654587548,-4.20129632948259,
-0.583071413770052));
#43532=CARTESIAN_POINT('Ctrl Pts',(-65.6507333595047,-3.41624951217949,
-2.51398138263055));
#43533=CARTESIAN_POINT('Ctrl Pts',(-65.5322012602546,-1.80619393837446,
-3.83777625437688));
#43534=CARTESIAN_POINT('Ctrl Pts',(-65.4136691610045,0.240049276229987,
-4.23476557399121));
#43535=CARTESIAN_POINT('Ctrl Pts',(-65.2951370617545,2.22832167981034,-3.60907822206265));
#43536=CARTESIAN_POINT('Ctrl Pts',(-65.1766049625043,3.6784645083721,-2.11181485512497));
#43537=CARTESIAN_POINT('Ctrl Pts',(-65.0580728632543,4.24027484861026,-0.104557782698988));
#43538=CARTESIAN_POINT('Ctrl Pts',(-64.9395407640041,3.77807805248247,1.92794951983446));
#43539=CARTESIAN_POINT('Ctrl Pts',(-64.8210086647541,2.4034925491091,3.4948657610925));
#43540=CARTESIAN_POINT('Ctrl Pts',(-64.7024765655039,0.448474500591471,
4.21778777844487));
#43541=CARTESIAN_POINT('Ctrl Pts',(-64.583944466254,-1.61484810493722,3.92213318484474));
#43542=CARTESIAN_POINT('Ctrl Pts',(-64.4654123670038,-3.2881922202403,2.67930122316078));
#43543=CARTESIAN_POINT('Ctrl Pts',(-64.3468802677538,-4.16745283400511,
0.789430172987094));
#43544=CARTESIAN_POINT('Ctrl Pts',(-64.2283481685037,-4.04029249751279,
-1.29108468204897));
#43545=CARTESIAN_POINT('Ctrl Pts',(-64.1098160692536,-2.93741985505644,
-3.05980844446182));
#43546=CARTESIAN_POINT('Ctrl Pts',(-63.9912839700035,-1.12517364567985,
-4.08960235093184));
#43547=CARTESIAN_POINT('Ctrl Pts',(-63.8727518707534,0.95879689383177,-4.13177584557272));
#43548=CARTESIAN_POINT('Ctrl Pts',(-63.7542197715033,2.81122233387158,-3.17614422078426));
#43549=CARTESIAN_POINT('Ctrl Pts',(-63.6356876722533,3.98475033575612,-1.45348817792618));
#43550=CARTESIAN_POINT('Ctrl Pts',(-63.5171555730031,4.1959792117271,0.620178664929396));
#43551=CARTESIAN_POINT('Ctrl Pts',(-63.3986234737531,3.39389814665504,2.54407517416668));
#43552=CARTESIAN_POINT('Ctrl Pts',(-63.2800913745029,1.77220607843935,3.85358907217963));
#43553=CARTESIAN_POINT('Ctrl Pts',(-63.1615592752529,-0.277465716615854,
4.23247869430933));
#43554=CARTESIAN_POINT('Ctrl Pts',(-63.0430271760028,-2.26013080006508,
3.58924391596298));
#43555=CARTESIAN_POINT('Ctrl Pts',(-62.9244950767527,-3.69698455028266,
2.07922301753555));
#43556=CARTESIAN_POINT('Ctrl Pts',(-62.8059629775026,-4.2410333060877,0.0670791945175098));
#43557=CARTESIAN_POINT('Ctrl Pts',(-62.6874308782525,-3.76089176148606,
-1.96126394961557));
#43558=CARTESIAN_POINT('Ctrl Pts',(-62.5688987790024,-2.37251192093704,
-3.51597074883963));
#43559=CARTESIAN_POINT('Ctrl Pts',(-62.4503666797524,-0.411181216372217,
-4.22158656537844));
#43560=CARTESIAN_POINT('Ctrl Pts',(-62.3318345805023,1.64944788626615,-3.90770838115492));
#43561=CARTESIAN_POINT('Ctrl Pts',(-62.2133024812522,3.3117428085009,-2.65013635349193));
#43562=CARTESIAN_POINT('Ctrl Pts',(-62.0947703820021,4.17426686894535,-0.752568421026256));
#43563=CARTESIAN_POINT('Ctrl Pts',(-61.976238282752,4.02872442070117,1.32674137044345));
#43564=CARTESIAN_POINT('Ctrl Pts',(-61.8577061835019,2.91026330437545,3.08564914085777));
#43565=CARTESIAN_POINT('Ctrl Pts',(-61.7391740842519,1.08898680526139,4.09938664434021));
#43566=CARTESIAN_POINT('Ctrl Pts',(-61.6206419850017,-0.995275066945756,
4.12314087364582));
#43567=CARTESIAN_POINT('Ctrl Pts',(-61.5021098857517,-2.83918252492348,
3.15117528982951));
#43568=CARTESIAN_POINT('Ctrl Pts',(-61.3835777865016,-3.99744028842169,
1.41821517194611));
#43569=CARTESIAN_POINT('Ctrl Pts',(-61.2650456872515,-4.19033435407454,
-0.657237475982055));
#43570=CARTESIAN_POINT('Ctrl Pts',(-61.1465135880014,-3.3712816981627,-2.57397025366613));
#43571=CARTESIAN_POINT('Ctrl Pts',(-61.0279814887513,-1.73807978469344,
-3.86910089790803));
#43572=CARTESIAN_POINT('Ctrl Pts',(-60.9094493895012,0.314860461962913,
-4.22986122300694));
#43573=CARTESIAN_POINT('Ctrl Pts',(-60.7909172902512,2.29176343348649,-3.56912927064055));
#43574=CARTESIAN_POINT('Ctrl Pts',(-60.672385191001,3.71521573733988,-2.04646876241471));
#43575=CARTESIAN_POINT('Ctrl Pts',(-60.553853091751,4.24146069462157,-0.0295953967523683));
#43576=CARTESIAN_POINT('Ctrl Pts',(-60.4353209925008,3.74341133987005,1.99442525015962));
#43577=CARTESIAN_POINT('Ctrl Pts',(-60.3167888932508,2.34134674152,3.53680099229865));
#43578=CARTESIAN_POINT('Ctrl Pts',(-60.1982567940007,0.373854285980798,
4.22505585861098));
#43579=CARTESIAN_POINT('Ctrl Pts',(-60.0797246947506,-1.68391575197083,
3.89297786596098));
#43580=CARTESIAN_POINT('Ctrl Pts',(-59.9611925955005,-3.33504093198254,
2.62076547651056));
#43581=CARTESIAN_POINT('Ctrl Pts',(-59.8426604962505,-4.18074236031188,
0.715645897712674));
#43582=CARTESIAN_POINT('Ctrl Pts',(-59.7241283970003,-4.0168668570281,-1.36229041980425));
#43583=CARTESIAN_POINT('Ctrl Pts',(-59.6055962977503,-2.88282865866802,
-3.11125693021052));
#43584=CARTESIAN_POINT('Ctrl Pts',(-59.4870641985001,-1.05281798849905,
-4.10883397176923));
#43585=CARTESIAN_POINT('Ctrl Pts',(-59.3685320992501,1.03189169588001,-4.11422147186713));
#43586=CARTESIAN_POINT('Ctrl Pts',(-59.28951069975,2.25480927425104,-3.45523440144076));
#43587=CARTESIAN_POINT('Ctrl Pts',(-59.25,2.75129702511905,-2.99988915288066));
#43588=CARTESIAN_POINT('Ctrl Pts',(-89.9038972033484,-1.91758108071826,
3.91047455474599));
#43589=CARTESIAN_POINT('Ctrl Pts',(-89.8643865035983,-2.56477256599302,
3.59311098917602));
#43590=CARTESIAN_POINT('Ctrl Pts',(-89.7853651040982,-3.69791038417238,
2.63117873038272));
#43591=CARTESIAN_POINT('Ctrl Pts',(-89.6668330048482,-4.5047299324047,0.551612640925381));
#43592=CARTESIAN_POINT('Ctrl Pts',(-89.5483009055982,-4.22357796578305,
-1.66068940373427));
#43593=CARTESIAN_POINT('Ctrl Pts',(-89.429768806348,-2.9225009322427,-3.47217295571325));
#43594=CARTESIAN_POINT('Ctrl Pts',(-89.3112367070979,-0.915628362002354,
-4.44502861127136));
#43595=CARTESIAN_POINT('Ctrl Pts',(-89.1927046078479,1.31235197600245,-4.34448653025811));
#43596=CARTESIAN_POINT('Ctrl Pts',(-89.0741725085977,3.22341138672613,-3.19474261450462));
#43597=CARTESIAN_POINT('Ctrl Pts',(-88.9556404093477,4.35602853470446,-1.27349677877322));
#43598=CARTESIAN_POINT('Ctrl Pts',(-88.8371083100975,4.43668606489078,0.955299664431044));
#43599=CARTESIAN_POINT('Ctrl Pts',(-88.7185762108476,3.44590329221712,2.95339214077506));
#43600=CARTESIAN_POINT('Ctrl Pts',(-88.6000441115973,1.62295088153958,4.23825551975466));
#43601=CARTESIAN_POINT('Ctrl Pts',(-88.4815120123475,-0.591936987748441,
4.4995985751017));
#43602=CARTESIAN_POINT('Ctrl Pts',(-88.3629799130971,-2.66387466866712,
3.67430941079818));
#43603=CARTESIAN_POINT('Ctrl Pts',(-88.2444478138472,-4.0924987495111,1.96169098685439));
#43604=CARTESIAN_POINT('Ctrl Pts',(-88.125915714597,-4.53280292882157,-0.224666806026332));
#43605=CARTESIAN_POINT('Ctrl Pts',(-88.007383615347,-3.87845577890968,-2.35676863603953));
#43606=CARTESIAN_POINT('Ctrl Pts',(-87.8888515160968,-2.28747915070016,
-3.91972150839504));
#43607=CARTESIAN_POINT('Ctrl Pts',(-87.7703194168468,-0.144086689434017,
-4.5360794342553));
#43608=CARTESIAN_POINT('Ctrl Pts',(-87.6517873175967,2.03410205493234,-4.05699475219311));
#43609=CARTESIAN_POINT('Ctrl Pts',(-87.5332552183467,3.72106438176611,-2.59816424856796));
#43610=CARTESIAN_POINT('Ctrl Pts',(-87.4147231190965,4.50940654448005,-0.511888866120898));
#43611=CARTESIAN_POINT('Ctrl Pts',(-87.2961910198465,4.20874748724988,1.69800535411033));
#43612=CARTESIAN_POINT('Ctrl Pts',(-87.1776589205963,2.89169500845528,3.49783898613552));
#43613=CARTESIAN_POINT('Ctrl Pts',(-87.0591268213463,0.876311305684017,
4.45296037370795));
#43614=CARTESIAN_POINT('Ctrl Pts',(-86.9405947220962,-1.35069760126606,
4.33271203572432));
#43615=CARTESIAN_POINT('Ctrl Pts',(-86.8220626228461,-3.25151916609637,
3.166133400059));
#43616=CARTESIAN_POINT('Ctrl Pts',(-86.703530523596,-4.36711360556095,1.2349479141299));
#43617=CARTESIAN_POINT('Ctrl Pts',(-86.5849984243459,-4.42806992436922,
-0.994471889693123));
#43618=CARTESIAN_POINT('Ctrl Pts',(-86.4664663250958,-3.41966744810485,
-2.98373124440774));
#43619=CARTESIAN_POINT('Ctrl Pts',(-86.3479342258457,-1.5854307993215,-4.25243304180721));
#43620=CARTESIAN_POINT('Ctrl Pts',(-86.2294021265957,0.631680193857936,
-4.49419155434812));
#43621=CARTESIAN_POINT('Ctrl Pts',(-86.1108700273456,2.69624328636905,-3.65062319819482));
#43622=CARTESIAN_POINT('Ctrl Pts',(-85.9923379280955,4.10967585899764,-1.92544590379988));
#43623=CARTESIAN_POINT('Ctrl Pts',(-85.8738058288454,4.53064035867955,0.264717839957676));
#43624=CARTESIAN_POINT('Ctrl Pts',(-85.7552737295953,3.85747576880117,2.39095342648068));
#43625=CARTESIAN_POINT('Ctrl Pts',(-85.6367416303453,2.25274828344074,3.93978460907987));
#43626=CARTESIAN_POINT('Ctrl Pts',(-85.5182095310951,0.103992309116789,
4.53717568473301));
#43627=CARTESIAN_POINT('Ctrl Pts',(-85.3996774318451,-2.06987733601028,
4.03885941923692));
#43628=CARTESIAN_POINT('Ctrl Pts',(-85.2811453325949,-3.74388099623042,
2.56517692967806));
#43629=CARTESIAN_POINT('Ctrl Pts',(-85.162613233345,-4.51375438312612,0.47201585068471));
#43630=CARTESIAN_POINT('Ctrl Pts',(-85.0440811340948,-4.19357656694023,
-1.73513491455207));
#43631=CARTESIAN_POINT('Ctrl Pts',(-84.9255490348447,-2.86066903752568,
-3.52325847082353));
#43632=CARTESIAN_POINT('Ctrl Pts',(-84.8070169355947,-0.836922915379946,
-4.46053109261663));
#43633=CARTESIAN_POINT('Ctrl Pts',(-84.6884848363446,1.38893629342528,-4.32060569449399));
#43634=CARTESIAN_POINT('Ctrl Pts',(-84.5699527370945,3.27937368944608,-3.13727362521293));
#43635=CARTESIAN_POINT('Ctrl Pts',(-84.4514206378443,4.37785721910273,-1.19630421032357));
#43636=CARTESIAN_POINT('Ctrl Pts',(-84.3328885385943,4.41910809417767,1.03356724331863));
#43637=CARTESIAN_POINT('Ctrl Pts',(-84.2143564393443,3.39316441550957,3.01383689734654));
#43638=CARTESIAN_POINT('Ctrl Pts',(-84.095824340094,1.54778692644035,4.26627861547135));
#43639=CARTESIAN_POINT('Ctrl Pts',(-83.9772922408442,-0.671374082526944,
4.48843340552124));
#43640=CARTESIAN_POINT('Ctrl Pts',(-83.8587601415938,-2.72840129681721,
3.6266518936912));
#43641=CARTESIAN_POINT('Ctrl Pts',(-83.7402280423439,-4.12653197761353,
1.88905040489152));
#43642=CARTESIAN_POINT('Ctrl Pts',(-83.6216959430938,-4.52812390929942,
-0.304748185423393));
#43643=CARTESIAN_POINT('Ctrl Pts',(-83.5031638438436,-3.8361944625323,-2.42495147170502));
#43644=CARTESIAN_POINT('Ctrl Pts',(-83.3846317445937,-2.21784145918652,
-3.95953998040192));
#43645=CARTESIAN_POINT('Ctrl Pts',(-83.2660996453435,-0.0638898065504608,
-4.53791754961532));
#43646=CARTESIAN_POINT('Ctrl Pts',(-83.1475675460934,2.10549094447769,-4.02040862067655));
#43647=CARTESIAN_POINT('Ctrl Pts',(-83.0290354468434,3.76640518574513,-2.53198925180974));
#43648=CARTESIAN_POINT('Ctrl Pts',(-82.9105033475932,4.51774966412024,-0.432105967129836));
#43649=CARTESIAN_POINT('Ctrl Pts',(-82.7919712483431,4.17807809718167,1.77212894799975));
#43650=CARTESIAN_POINT('Ctrl Pts',(-82.6734391490932,2.82941962713926,3.54840276294096));
#43651=CARTESIAN_POINT('Ctrl Pts',(-82.5549070498429,0.797469155184746,
4.46775341094568));
#43652=CARTESIAN_POINT('Ctrl Pts',(-82.436374950593,-1.42706649935728,4.3081618819283));
#43653=CARTESIAN_POINT('Ctrl Pts',(-82.3178428513427,-3.30697206939204,
3.1081688060253));
#43654=CARTESIAN_POINT('Ctrl Pts',(-82.1993107520927,-4.38825888952899,
1.15756706628934));
#43655=CARTESIAN_POINT('Ctrl Pts',(-82.0807786528427,-4.40980109887219,
-1.07258186767885));
#43656=CARTESIAN_POINT('Ctrl Pts',(-81.9622465535925,-3.36639635160963,
-3.04370714727242));
#43657=CARTESIAN_POINT('Ctrl Pts',(-81.8437144543425,-1.51002215992195,
-4.2797909611373));
#43658=CARTESIAN_POINT('Ctrl Pts',(-81.7251823550924,0.711015531901254,
-4.48232467675905));
#43659=CARTESIAN_POINT('Ctrl Pts',(-81.6066502558422,2.76034619889032,-3.60239732077954));
#43660=CARTESIAN_POINT('Ctrl Pts',(-81.4881181565923,4.14306578347967,-1.8525073571373));
#43661=CARTESIAN_POINT('Ctrl Pts',(-81.3695860573421,4.52525377986144,0.344754727795806));
#43662=CARTESIAN_POINT('Ctrl Pts',(-81.251053958092,3.81461352102674,2.458760110236));
#43663=CARTESIAN_POINT('Ctrl Pts',(-81.132521858842,2.18276140506687,3.97898608228761));
#43664=CARTESIAN_POINT('Ctrl Pts',(-81.0139897595918,0.0237823137164571,
4.53830496948386));
#43665=CARTESIAN_POINT('Ctrl Pts',(-80.8954576603418,-2.14094009848806,
4.00164379838764));
#43666=CARTESIAN_POINT('Ctrl Pts',(-80.7769255610918,-3.78863519108316,
2.49860380680357));
#43667=CARTESIAN_POINT('Ctrl Pts',(-80.6583934618415,-4.52139207536215,
0.392162332894574));
#43668=CARTESIAN_POINT('Ctrl Pts',(-80.5398613625916,-4.16225328853891,
-1.80898456503483));
#43669=CARTESIAN_POINT('Ctrl Pts',(-80.4213292633414,-2.79794921809744,
-3.57326989848707));
#43670=CARTESIAN_POINT('Ctrl Pts',(-80.3027971640913,-0.75795310673366,
-4.47462676460175));
#43671=CARTESIAN_POINT('Ctrl Pts',(-80.1842650648413,1.46508524081083,-4.29538156996789));
#43672=CARTESIAN_POINT('Ctrl Pts',(-80.0657329655912,3.3343121502984,-3.07882121580877));
#43673=CARTESIAN_POINT('Ctrl Pts',(-79.9472008663411,4.39831780438567,-1.1187395076727));
#43674=CARTESIAN_POINT('Ctrl Pts',(-79.828668767091,4.400149665412,1.11151271542078));
#43675=CARTESIAN_POINT('Ctrl Pts',(-79.7101366678409,3.33936534716099,3.07333966113867));
#43676=CARTESIAN_POINT('Ctrl Pts',(-79.5916045685908,1.4721394495319,4.2929690233084));
#43677=CARTESIAN_POINT('Ctrl Pts',(-79.4730724693408,-0.750601445805186,
4.47586584536369));
#43678=CARTESIAN_POINT('Ctrl Pts',(-79.3545403700905,-2.79207549722183,
3.57786137358953));
#43679=CARTESIAN_POINT('Ctrl Pts',(-79.2360082708406,-4.15927598565198,
1.81581961548961));
#43680=CARTESIAN_POINT('Ctrl Pts',(-79.1174761715905,-4.5220301935998,-0.384734343615344));
#43681=CARTESIAN_POINT('Ctrl Pts',(-78.9989440723404,-3.79273463181798,
-2.4923766986529));
#43682=CARTESIAN_POINT('Ctrl Pts',(-78.8804119730903,-2.14751085726326,
-3.99812140132146));
#43683=CARTESIAN_POINT('Ctrl Pts',(-78.7618798738402,0.0163270289763692,
-4.5383379030618));
#43684=CARTESIAN_POINT('Ctrl Pts',(-78.6433477745902,2.17622204474192,-3.98256644023163));
#43685=CARTESIAN_POINT('Ctrl Pts',(-78.52481567534,3.81056924461044,-2.46502315761527));
#43686=CARTESIAN_POINT('Ctrl Pts',(-78.4062835760899,4.52468139540959,-0.35218815789933));
#43687=CARTESIAN_POINT('Ctrl Pts',(-78.2877514768399,4.1461032500353,1.84569906829402));
#43688=CARTESIAN_POINT('Ctrl Pts',(-78.1692193775898,2.76626052430319,3.59785756990614));
#43689=CARTESIAN_POINT('Ctrl Pts',(-78.0506872783397,0.718377341221213,
4.48115135241873));
#43690=CARTESIAN_POINT('Ctrl Pts',(-77.9321551790897,-1.50298851030343,
4.28226427499296));
#43691=CARTESIAN_POINT('Ctrl Pts',(-77.8136230798394,-3.3613938873463,3.04923613162936));
#43692=CARTESIAN_POINT('Ctrl Pts',(-77.6950909805895,-4.40802896695736,
1.07981855511509));
#43693=CARTESIAN_POINT('Ctrl Pts',(-77.5765588813393,-4.39016302965047,
-1.15034463604321));
#43694=CARTESIAN_POINT('Ctrl Pts',(-77.4580267820892,-3.31205642877169,
-3.10275651618137));
#43695=CARTESIAN_POINT('Ctrl Pts',(-77.3394946828392,-1.43417616674434,
-4.30576264206103));
#43696=CARTESIAN_POINT('Ctrl Pts',(-77.2209625835891,0.790198047099194,
-4.46915637620211));
#43697=CARTESIAN_POINT('Ctrl Pts',(-77.102430484339,2.82344709756949,-3.55284663971428));
#43698=CARTESIAN_POINT('Ctrl Pts',(-76.983898385089,4.17544253569911,-1.77939153711507));
#43699=CARTESIAN_POINT('Ctrl Pts',(-76.8653662858387,4.51788697953528,0.425492568419178));
#43700=CARTESIAN_POINT('Ctrl Pts',(-76.7468341865888,3.77170020986389,2.52417031947069));
#43701=CARTESIAN_POINT('Ctrl Pts',(-76.6283020873386,2.10979798242572,4.02021622200475));
#43702=CARTESIAN_POINT('Ctrl Pts',(-76.5097699880885,-0.0518487682622708,
4.53152423158982));
#43703=CARTESIAN_POINT('Ctrl Pts',(-76.3517271890885,-2.94243730562177,
3.78859930032371));
#43704=CARTESIAN_POINT('Ctrl Pts',(-76.1541736903383,-5.12736172522327,
0.359976101474219));
#43705=CARTESIAN_POINT('Ctrl Pts',(-75.9171094918381,-3.09694643473724,
-4.10548315491292));
#43706=CARTESIAN_POINT('Ctrl Pts',(-75.6800452933379,1.7450843387911,-4.83295838873338));
#43707=CARTESIAN_POINT('Ctrl Pts',(-75.4429810948378,5.00285271579571,-1.17963732083592));
#43708=CARTESIAN_POINT('Ctrl Pts',(-75.2059168963375,3.71989551972808,3.54743426964955));
#43709=CARTESIAN_POINT('Ctrl Pts',(-74.9688526978376,-0.939579108086353,
5.05306947513863));
#43710=CARTESIAN_POINT('Ctrl Pts',(-74.7317884993371,-4.74613568087871,
1.97302396061139));
#43711=CARTESIAN_POINT('Ctrl Pts',(-74.4947243008372,-4.24493582968068,
-2.89824681684524));
#43712=CARTESIAN_POINT('Ctrl Pts',(-74.2576601023368,0.109449407841399,
-5.138739950375));
#43713=CARTESIAN_POINT('Ctrl Pts',(-74.0205959038369,4.36408416590106,-2.71497503006226));
#43714=CARTESIAN_POINT('Ctrl Pts',(-73.7835317053365,4.6583847905374,2.17286992672524));
#43715=CARTESIAN_POINT('Ctrl Pts',(-73.5464675068365,0.722948980038282,
5.08895119616166));
#43716=CARTESIAN_POINT('Ctrl Pts',(-73.3094033083362,-3.86578692129527,
3.38504026798275));
#43717=CARTESIAN_POINT('Ctrl Pts',(-73.0723391098361,-4.95130148340585,
-1.38949011343312));
#43718=CARTESIAN_POINT('Ctrl Pts',(-72.8352749113358,-1.53167950267415,
-4.90646297815493));
#43719=CARTESIAN_POINT('Ctrl Pts',(-72.6377214125857,2.4571454286763,-4.11993425897348));
#43720=CARTESIAN_POINT('Ctrl Pts',(-72.4796786135857,4.20157589201124,-1.69828153729762));
#43721=CARTESIAN_POINT('Ctrl Pts',(-72.3611465143355,4.51245306445273,0.50115201229658));
#43722=CARTESIAN_POINT('Ctrl Pts',(-72.2426144150855,3.72422628860401,2.59370330339747));
#43723=CARTESIAN_POINT('Ctrl Pts',(-72.1240823158353,2.04131079620884,4.05282579429657));
#43724=CARTESIAN_POINT('Ctrl Pts',(-72.0055502165853,-0.136906442683483,
4.53671811304536));
#43725=CARTESIAN_POINT('Ctrl Pts',(-71.8870181173352,-2.28090218001176,
3.92327133949721));
#43726=CARTESIAN_POINT('Ctrl Pts',(-71.7684860180852,-3.87464592062427,
2.36323732586829));
#43727=CARTESIAN_POINT('Ctrl Pts',(-71.6499539188349,-4.53239451861189,
0.232062781769669));
#43728=CARTESIAN_POINT('Ctrl Pts',(-71.531421819585,-4.09573226279255,-1.95494066856108));
#43729=CARTESIAN_POINT('Ctrl Pts',(-71.4128897203348,-2.66989882164255,
-3.66994066583849));
#43730=CARTESIAN_POINT('Ctrl Pts',(-71.2943576210847,-0.599331894321411,
-4.49861409391326));
#43731=CARTESIAN_POINT('Ctrl Pts',(-71.1758255218347,1.61598832509741,-4.24091871950784));
#43732=CARTESIAN_POINT('Ctrl Pts',(-71.0572934225845,3.44104607812029,-2.95904776427113));
#43733=CARTESIAN_POINT('Ctrl Pts',(-70.9387613233345,4.43511109512073,-0.962586630699401));
#43734=CARTESIAN_POINT('Ctrl Pts',(-70.8202292240844,4.35811478205403,1.26633799915005));
#43735=CARTESIAN_POINT('Ctrl Pts',(-70.7016971248343,3.22865457797459,3.18944616301615));
#43736=CARTESIAN_POINT('Ctrl Pts',(-70.5831650255842,1.3194884192469,4.34231833701809));
#43737=CARTESIAN_POINT('Ctrl Pts',(-70.4646329263342,-0.90832794582209,
4.44653994453993));
#43738=CARTESIAN_POINT('Ctrl Pts',(-70.3461008270841,-2.91678736241942,
3.47694252487875));
#43739=CARTESIAN_POINT('Ctrl Pts',(-70.227568727834,-4.22085580138227,1.6676791652414));
#43740=CARTESIAN_POINT('Ctrl Pts',(-70.1090366285839,-4.50560674758229,
-0.544321098166527));
#43741=CARTESIAN_POINT('Ctrl Pts',(-69.9905045293338,-3.70227409192413,
-2.62487030987185));
#43742=CARTESIAN_POINT('Ctrl Pts',(-69.8719724300837,-2.00485904938691,
-4.0715252398919));
#43743=CARTESIAN_POINT('Ctrl Pts',(-69.7534403308337,0.176720360740206,
-4.53492530422694));
#43744=CARTESIAN_POINT('Ctrl Pts',(-69.6349082315836,2.31562260365669,-3.90316148118993));
#43745=CARTESIAN_POINT('Ctrl Pts',(-69.5163761323335,3.89531249551915,-2.32880187186253));
#43746=CARTESIAN_POINT('Ctrl Pts',(-69.3978440330833,4.53430209359898,-0.192047176332951));
#43747=CARTESIAN_POINT('Ctrl Pts',(-69.2793119338334,4.07827830998647,1.99108604054206));
#43748=CARTESIAN_POINT('Ctrl Pts',(-69.1607798345831,2.63736881893472,3.69338101303916));
#43749=CARTESIAN_POINT('Ctrl Pts',(-69.0422477353331,0.559546724810547,
4.50374122892928));
#43750=CARTESIAN_POINT('Ctrl Pts',(-68.9237156360831,-1.65340336452998,
4.22646837308677));
#43751=CARTESIAN_POINT('Ctrl Pts',(-68.8051835368329,-3.46706404337724,
2.92852258205094));
#43752=CARTESIAN_POINT('Ctrl Pts',(-68.6866514375829,-4.44344448700827,
0.923351875166453));
#43753=CARTESIAN_POINT('Ctrl Pts',(-68.5681193383327,-4.34675324844664,
-1.3048041200136));
#43754=CARTESIAN_POINT('Ctrl Pts',(-68.4495872390827,-3.20034082308918,
-3.21785584054912));
#43755=CARTESIAN_POINT('Ctrl Pts',(-68.3310551398326,-1.28106060999283,
-4.35380997610297));
#43756=CARTESIAN_POINT('Ctrl Pts',(-68.2125230405825,0.947589927807374,
-4.43833875714834));
#43757=CARTESIAN_POINT('Ctrl Pts',(-68.0939909413324,2.94740179758105,-3.45102886659968));
#43758=CARTESIAN_POINT('Ctrl Pts',(-67.9754588420823,4.23542950660619,-1.63031116326222));
#43759=CARTESIAN_POINT('Ctrl Pts',(-67.8569267428322,4.50062020737443,0.584119288725105));
#43760=CARTESIAN_POINT('Ctrl Pts',(-67.7383946435822,3.6789315489109,2.65748758283382));
#43761=CARTESIAN_POINT('Ctrl Pts',(-67.6198625443321,1.96879761395276,4.08908468361586));
#43762=CARTESIAN_POINT('Ctrl Pts',(-67.5013304450819,-0.216792011668601,
4.53318638687673));
#43763=CARTESIAN_POINT('Ctrl Pts',(-67.382798345832,-2.35002735013129,3.88254414631988));
#43764=CARTESIAN_POINT('Ctrl Pts',(-67.2642662465817,-3.91574174641298,
2.29428511085401));
#43765=CARTESIAN_POINT('Ctrl Pts',(-67.1457341473317,-4.53582227799202,
0.151966631071091));
#43766=CARTESIAN_POINT('Ctrl Pts',(-67.0272020480817,-4.06052231000895,
-2.02705110059108));
#43767=CARTESIAN_POINT('Ctrl Pts',(-66.9086699488315,-2.60462462813354,
-3.71654518888283));
#43768=CARTESIAN_POINT('Ctrl Pts',(-66.7901378495815,-0.51972191663431,
-4.50851047729267));
#43769=CARTESIAN_POINT('Ctrl Pts',(-66.6716057503314,1.69069127957646,-4.21169094208632));
#43770=CARTESIAN_POINT('Ctrl Pts',(-66.5530736510813,3.49281020301257,-2.89776715424464));
#43771=CARTESIAN_POINT('Ctrl Pts',(-66.4345415518312,4.45143131049253,-0.884045746810973));
#43772=CARTESIAN_POINT('Ctrl Pts',(-66.3160094525812,4.3350519541509,1.34316869726045));
#43773=CARTESIAN_POINT('Ctrl Pts',(-66.197477353331,3.17177722049131,3.24601399535804));
#43774=CARTESIAN_POINT('Ctrl Pts',(-66.078945254081,1.24253267951826,4.36496164184945));
#43775=CARTESIAN_POINT('Ctrl Pts',(-65.9604131548308,-0.986777865763803,
4.42979085715414));
#43776=CARTESIAN_POINT('Ctrl Pts',(-65.8418810555808,-2.9777860338117,3.42484567992835));
#43777=CARTESIAN_POINT('Ctrl Pts',(-65.7233489563307,-4.2496723859251,1.59281581069298));
#43778=CARTESIAN_POINT('Ctrl Pts',(-65.6048168570806,-4.49528213905086,
-0.623871849676049));
#43779=CARTESIAN_POINT('Ctrl Pts',(-65.4862847578305,-3.65530165222434,
-2.68989728906772));
#43780=CARTESIAN_POINT('Ctrl Pts',(-65.3677526585804,-1.93258240173615,
-4.10632473813112));
#43781=CARTESIAN_POINT('Ctrl Pts',(-65.2492205593303,0.25684672998572,-4.53109339473195));
#43782=CARTESIAN_POINT('Ctrl Pts',(-65.1306884600803,2.38424854181727,-3.8616235556214));
#43783=CARTESIAN_POINT('Ctrl Pts',(-65.0121563608302,3.93586514894891,-2.25958914933163));
#43784=CARTESIAN_POINT('Ctrl Pts',(-64.8936242615801,4.53698818097217,-0.111874216005024));
#43785=CARTESIAN_POINT('Ctrl Pts',(-64.7750921623301,4.04244915315367,2.06285783287529));
#43786=CARTESIAN_POINT('Ctrl Pts',(-64.6565600630799,2.57167699681937,3.73941907500589));
#43787=CARTESIAN_POINT('Ctrl Pts',(-64.5380279638298,0.479856514328996,
4.51292757754252));
#43788=CARTESIAN_POINT('Ctrl Pts',(-64.4194958645798,-1.72784713909916,
4.19658454679454));
#43789=CARTESIAN_POINT('Ctrl Pts',(-64.3009637653296,-3.51828354826676,
2.86678538933129));
#43790=CARTESIAN_POINT('Ctrl Pts',(-64.1824316660796,-4.45907044418055,
0.844670567927753));
#43791=CARTESIAN_POINT('Ctrl Pts',(-64.0638995668294,-4.3230120601484,-1.38142836307181));
#43792=CARTESIAN_POINT('Ctrl Pts',(-63.9453674675794,-3.14296587857083,
-3.27391861240125));
#43793=CARTESIAN_POINT('Ctrl Pts',(-63.8268353683293,-1.20390769802672,
-4.37577237172135));
#43794=CARTESIAN_POINT('Ctrl Pts',(-63.7083032690792,1.02588872905094,-4.42089695764265));
#43795=CARTESIAN_POINT('Ctrl Pts',(-63.5897711698291,3.00793768286991,-3.39839498741083));
#43796=CARTESIAN_POINT('Ctrl Pts',(-63.4712390705791,4.26358333431514,-1.55519604739662));
#43797=CARTESIAN_POINT('Ctrl Pts',(-63.3527069713289,4.48959295585525,0.663575681608901));
#43798=CARTESIAN_POINT('Ctrl Pts',(-63.2341748720788,3.63138624937108,2.7220968943751));
#43799=CARTESIAN_POINT('Ctrl Pts',(-63.1156427728288,1.8962162405019,4.1232440582319));
#43800=CARTESIAN_POINT('Ctrl Pts',(-62.9971106735786,-0.296881386668499,
4.52864649059049));
#43801=CARTESIAN_POINT('Ctrl Pts',(-62.8785785743287,-2.41828350601072,
3.84040134348544));
#43802=CARTESIAN_POINT('Ctrl Pts',(-62.7600464750784,-3.95568113122819,
2.22471669713957));
#43803=CARTESIAN_POINT('Ctrl Pts',(-62.6415143758285,-4.53779971152945,
0.0717730627331741));
#43804=CARTESIAN_POINT('Ctrl Pts',(-62.5229822765783,-4.02406025104017,
-2.09850344066467));
#43805=CARTESIAN_POINT('Ctrl Pts',(-62.4044501773283,-2.53852849846159,
-3.7620008847675));
#43806=CARTESIAN_POINT('Ctrl Pts',(-62.2859180780781,-0.439953631668492,
-4.5169921846812));
#43807=CARTESIAN_POINT('Ctrl Pts',(-62.1673859788281,1.76486804094118,-4.18115036712692));
#43808=CARTESIAN_POINT('Ctrl Pts',(-62.048853879578,3.54348208949535,-2.83557970722072));
#43809=CARTESIAN_POINT('Ctrl Pts',(-61.9303217803279,4.46636129137614,-0.805229414005605));
#43810=CARTESIAN_POINT('Ctrl Pts',(-61.8117896810778,4.31063450688954,1.41958012907617));
#43811=CARTESIAN_POINT('Ctrl Pts',(-61.6932575818278,3.11390904761658,3.30156751213588));
#43812=CARTESIAN_POINT('Ctrl Pts',(-61.5747254825776,1.16518868259802,4.38624132129133));
#43813=CARTESIAN_POINT('Ctrl Pts',(-61.4561933833276,-1.06491946318739,
4.41165775335188));
#43814=CARTESIAN_POINT('Ctrl Pts',(-61.3376612840774,-3.03785438894894,
3.37167885492467));
#43815=CARTESIAN_POINT('Ctrl Pts',(-61.2191291848274,-4.27716126671725,
1.51745481199265));
#43816=CARTESIAN_POINT('Ctrl Pts',(-61.1005970855773,-4.48355309915555,
-0.703227683837457));
#43817=CARTESIAN_POINT('Ctrl Pts',(-60.9820649863272,-3.60718721436302,
-2.75408388276636));
#43818=CARTESIAN_POINT('Ctrl Pts',(-60.8635328870771,-1.85970195854767,
-4.13984132433085));
#43819=CARTESIAN_POINT('Ctrl Pts',(-60.745000787827,0.336892830201615,-4.52584586167209));
#43820=CARTESIAN_POINT('Ctrl Pts',(-60.6264686885769,2.45212963370055,-3.81887917538301));
#43821=CARTESIAN_POINT('Ctrl Pts',(-60.5079365893269,3.97518804602896,-2.1896704622455));
#43822=CARTESIAN_POINT('Ctrl Pts',(-60.3894044900767,4.53825700658604,-0.0316663353369214));
#43823=CARTESIAN_POINT('Ctrl Pts',(-60.2708723908267,4.00535663651003,2.13398520399503));
#43824=CARTESIAN_POINT('Ctrl Pts',(-60.1523402915766,2.50518253488111,3.78428872500298));
#43825=CARTESIAN_POINT('Ctrl Pts',(-60.0338081923265,0.40001474844413,4.52070424178939));
#43826=CARTESIAN_POINT('Ctrl Pts',(-59.9152760930764,-1.80174779636003,
4.16538908378548));
#43827=CARTESIAN_POINT('Ctrl Pts',(-59.7967439938263,-3.56841049971614,
2.80415360243109));
#43828=CARTESIAN_POINT('Ctrl Pts',(-59.6782118945762,-4.47328990540352,
0.765723236253875));
#43829=CARTESIAN_POINT('Ctrl Pts',(-59.5596797953262,-4.29794720991927,
-1.45761672400295));
#43830=CARTESIAN_POINT('Ctrl Pts',(-59.4411476960761,-3.08455466192987,
-3.32896720715149));
#43831=CARTESIAN_POINT('Ctrl Pts',(-59.322615596826,-1.12648895203119,-4.39634972567962));
#43832=CARTESIAN_POINT('Ctrl Pts',(-59.2040834975759,1.1040983415934,-4.40211421622372));
#43833=CARTESIAN_POINT('Ctrl Pts',(-59.1250620980759,2.41258960630257,-3.6970145100295));
#43834=CARTESIAN_POINT('Ctrl Pts',(-59.0855513983258,2.94381909922657,-3.20980646698104));
#43835=CARTESIAN_POINT('Ctrl Pts',(-89.7394486016742,-2.04298847651448,
4.16621468233137));
#43836=CARTESIAN_POINT('Ctrl Pts',(-89.6999379019242,-2.73250547259342,
3.82809593791711));
#43837=CARTESIAN_POINT('Ctrl Pts',(-89.6209165024241,-3.93974908180555,
2.80325451678348));
#43838=CARTESIAN_POINT('Ctrl Pts',(-89.502384403174,-4.79933361579976,0.587687415276454));
#43839=CARTESIAN_POINT('Ctrl Pts',(-89.3838523039239,-4.49979466345347,
-1.76929640629746));
#43840=CARTESIAN_POINT('Ctrl Pts',(-89.2653202046738,-3.11362882498736,
-3.69924870886316));
#43841=CARTESIAN_POINT('Ctrl Pts',(-89.1467881054238,-0.975509307611675,
-4.73572790319936));
#43842=CARTESIAN_POINT('Ctrl Pts',(-89.0282560061737,1.3981781480133,-4.62861049628486));
#43843=CARTESIAN_POINT('Ctrl Pts',(-88.9097239069235,3.43421844550137,-3.40367477156069));
#43844=CARTESIAN_POINT('Ctrl Pts',(-88.7911918076735,4.64090733333486,-1.35678186965505));
#43845=CARTESIAN_POINT('Ctrl Pts',(-88.6726597084234,4.72683976475678,1.01777506342507));
#43846=CARTESIAN_POINT('Ctrl Pts',(-88.5541276091732,3.67126104234722,3.14654027978409));
#43847=CARTESIAN_POINT('Ctrl Pts',(-88.4355955099233,1.72908983211939,4.51543211103203));
#43848=CARTESIAN_POINT('Ctrl Pts',(-88.3170634106731,-0.630648923767926,
4.79386667416986));
#43849=CARTESIAN_POINT('Ctrl Pts',(-88.198531311423,-2.83808872839281,3.91460463439585));
#43850=CARTESIAN_POINT('Ctrl Pts',(-88.0799992121731,-4.36014303096349,
2.08998311514671));
#43851=CARTESIAN_POINT('Ctrl Pts',(-87.9614671129227,-4.82924255094602,
-0.239359733146274));
#43852=CARTESIAN_POINT('Ctrl Pts',(-87.8429350136729,-4.13210191874425,
-2.51089834670044));
#43853=CARTESIAN_POINT('Ctrl Pts',(-87.7244029144226,-2.43707741598974,
-4.17606637514258));
#43854=CARTESIAN_POINT('Ctrl Pts',(-87.6058708151727,-0.153509778070305,
-4.83273333572255));
#43855=CARTESIAN_POINT('Ctrl Pts',(-87.4873387159224,2.16712977618899,-4.32231711678435));
#43856=CARTESIAN_POINT('Ctrl Pts',(-87.3688066166725,3.9644173217798,-2.7680809292967));
#43857=CARTESIAN_POINT('Ctrl Pts',(-87.2502745174223,4.80431607243491,-0.545365755459693));
#43858=CARTESIAN_POINT('Ctrl Pts',(-87.1317424181723,4.48399429023895,1.80905277299039));
#43859=CARTESIAN_POINT('Ctrl Pts',(-87.0132103189222,3.08080823245079,3.72659326545992));
#43860=CARTESIAN_POINT('Ctrl Pts',(-86.8946782196721,0.933620965159556,
4.74417839294364));
#43861=CARTESIAN_POINT('Ctrl Pts',(-86.7761461204221,-1.43903152903902,
4.61606596458752));
#43862=CARTESIAN_POINT('Ctrl Pts',(-86.6576140211718,-3.46416443836248,
3.37319455039963));
#43863=CARTESIAN_POINT('Ctrl Pts',(-86.5390819219218,-4.65271735391176,
1.31571195764929));
#43864=CARTESIAN_POINT('Ctrl Pts',(-86.4205498226717,-4.71766013945981,
-1.05950910305164));
#43865=CARTESIAN_POINT('Ctrl Pts',(-86.3020177234217,-3.64330940696034,
-3.17886352271374));
#43866=CARTESIAN_POINT('Ctrl Pts',(-86.1834856241716,-1.68911598361819,
-4.53053682523168));
#43867=CARTESIAN_POINT('Ctrl Pts',(-86.0649535249214,0.672991285672667,
-4.7881060410457));
#43868=CARTESIAN_POINT('Ctrl Pts',(-85.9464214256714,2.87257421306444,-3.88936937321837));
#43869=CARTESIAN_POINT('Ctrl Pts',(-85.8278893264213,4.37844350185034,-2.05136764915404));
#43870=CARTESIAN_POINT('Ctrl Pts',(-85.7093572271713,4.82693855143109,0.282030054426027));
#43871=CARTESIAN_POINT('Ctrl Pts',(-85.5908251279211,4.10974984230804,2.54731877952885));
#43872=CARTESIAN_POINT('Ctrl Pts',(-85.4722930286711,2.40007519360456,4.19744157742968));
#43873=CARTESIAN_POINT('Ctrl Pts',(-85.353760929421,0.110793275605439,4.83390127960553));
#43874=CARTESIAN_POINT('Ctrl Pts',(-85.2352288301709,-2.20524471574551,
4.30299575581568));
#43875=CARTESIAN_POINT('Ctrl Pts',(-85.1166967309208,-3.98872611419144,
2.73293628115596));
#43876=CARTESIAN_POINT('Ctrl Pts',(-84.9981646316707,-4.80894825427117,
0.502885094861233));
#43877=CARTESIAN_POINT('Ctrl Pts',(-84.8796325324206,-4.46783121078307,
-1.84861056008126));
#43878=CARTESIAN_POINT('Ctrl Pts',(-84.7611004331705,-3.04775320196515,
-3.75367515254084));
#43879=CARTESIAN_POINT('Ctrl Pts',(-84.6425683339205,-0.891656623568571,
-4.75224422736644));
#43880=CARTESIAN_POINT('Ctrl Pts',(-84.5240362346703,1.47977098366955,-4.60316788383619));
#43881=CARTESIAN_POINT('Ctrl Pts',(-84.4055041354203,3.49384061257721,-3.34244738250244));
#43882=CARTESIAN_POINT('Ctrl Pts',(-84.2869720361702,4.66416358629416,-1.2745410041183));
#43883=CARTESIAN_POINT('Ctrl Pts',(-84.1684399369201,4.70811221682231,1.1011612437331));
#43884=CARTESIAN_POINT('Ctrl Pts',(-84.0499078376701,3.61507310929904,3.21093804756714));
#43885=CARTESIAN_POINT('Ctrl Pts',(-83.9313757384199,1.64901024869993,4.54528788203497));
#43886=CARTESIAN_POINT('Ctrl Pts',(-83.8128436391698,-0.715281104838201,
4.78197131651296));
#43887=CARTESIAN_POINT('Ctrl Pts',(-83.6943115399198,-2.90683531703227,
3.86383037548819));
#43888=CARTESIAN_POINT('Ctrl Pts',(-83.5757794406696,-4.39640198946648,
2.01259193029946));
#43889=CARTESIAN_POINT('Ctrl Pts',(-83.4572473414197,-4.82425752942006,
-0.324678334240465));
#43890=CARTESIAN_POINT('Ctrl Pts',(-83.3387152421694,-4.08707676532076,
-2.58354025423768));
#43891=CARTESIAN_POINT('Ctrl Pts',(-83.2201831429194,-2.36288550685798,
-4.21848892523991));
#43892=CARTESIAN_POINT('Ctrl Pts',(-83.1016510436693,-0.0680681197065716,
-4.83469166151999));
#43893=CARTESIAN_POINT('Ctrl Pts',(-82.9831189444192,2.24318740950569,-4.28333829818827));
#43894=CARTESIAN_POINT('Ctrl Pts',(-82.8645868451692,4.01272335742881,-2.6975781708111));
#43895=CARTESIAN_POINT('Ctrl Pts',(-82.7460547459191,4.81320482162757,-0.460365155015403));
#43896=CARTESIAN_POINT('Ctrl Pts',(-82.6275226466689,4.45131916055545,1.88802395688276));
#43897=CARTESIAN_POINT('Ctrl Pts',(-82.508990547419,3.01446011936265,3.78046384980249));
#43898=CARTESIAN_POINT('Ctrl Pts',(-82.3904584481687,0.849622636977626,
4.75993887624899));
#43899=CARTESIAN_POINT('Ctrl Pts',(-82.2719263489188,-1.52039485720976,
4.58991026154776));
#43900=CARTESIAN_POINT('Ctrl Pts',(-82.1533942496686,-3.52324389193109,
3.31143914467132));
#43901=CARTESIAN_POINT('Ctrl Pts',(-82.0348621504185,-4.67524551291046,
1.23327049948577));
#43902=CARTESIAN_POINT('Ctrl Pts',(-81.9163300511685,-4.69819655570569,
-1.14272737555664));
#43903=CARTESIAN_POINT('Ctrl Pts',(-81.7977979519183,-3.58655444761841,
-3.24276177434604));
#43904=CARTESIAN_POINT('Ctrl Pts',(-81.6792658526683,-1.60877571385228,
-4.55968391814722));
#43905=CARTESIAN_POINT('Ctrl Pts',(-81.5607337534183,0.757515055244992,
-4.7754630845572));
#43906=CARTESIAN_POINT('Ctrl Pts',(-81.442201654168,2.9408693756048,-3.83798958395162));
#43907=CARTESIAN_POINT('Ctrl Pts',(-81.3236695549181,4.4140170854836,-1.97365901308971));
#43908=CARTESIAN_POINT('Ctrl Pts',(-81.2051374556679,4.82119969711933,0.367301254269179));
#43909=CARTESIAN_POINT('Ctrl Pts',(-81.0866053564178,4.06408445732841,2.61955993529313));
#43910=CARTESIAN_POINT('Ctrl Pts',(-80.9680732571678,2.32551126123019,4.23920677778083));
#43911=CARTESIAN_POINT('Ctrl Pts',(-80.8495411579176,0.0253376471827901,
4.83510441816165));
#43912=CARTESIAN_POINT('Ctrl Pts',(-80.7310090586676,-2.28095489369376,
4.26334628007464));
#43913=CARTESIAN_POINT('Ctrl Pts',(-80.6124769594175,-4.03640717721361,
2.66200935960581));
#43914=CARTESIAN_POINT('Ctrl Pts',(-80.4939448601674,-4.81708544199286,
0.417809257237047));
#43915=CARTESIAN_POINT('Ctrl Pts',(-80.3754127609174,-4.43445942929022,
-1.92728988501201));
#43916=CARTESIAN_POINT('Ctrl Pts',(-80.2568806616671,-2.98093158507008,
-3.80695726480094));
#43917=CARTESIAN_POINT('Ctrl Pts',(-80.1383485624172,-0.807522288557044,
-4.76726173860696));
#43918=CARTESIAN_POINT('Ctrl Pts',(-80.019816463167,1.56089997663453,-4.57629413322656));
#43919=CARTESIAN_POINT('Ctrl Pts',(-79.901284363917,3.55237197981238,-3.28017225889073));
#43920=CARTESIAN_POINT('Ctrl Pts',(-79.7827522646669,4.68596226817316,-1.19190366727064));
#43921=CARTESIAN_POINT('Ctrl Pts',(-79.6642201654169,4.68791393061135,1.18420425187621));
#43922=CARTESIAN_POINT('Ctrl Pts',(-79.5456880661667,3.55775564940722,3.27433221742542));
#43923=CARTESIAN_POINT('Ctrl Pts',(-79.4271559669167,1.56841552175181,4.57372380904366));
#43924=CARTESIAN_POINT('Ctrl Pts',(-79.3086238676665,-0.799689838231343,
4.76858185369549));
#43925=CARTESIAN_POINT('Ctrl Pts',(-79.1900917684164,-2.97467373022166,
3.81184901661207));
#43926=CARTESIAN_POINT('Ctrl Pts',(-79.0715596691664,-4.43128741453147,
1.93457193918746));
#43927=CARTESIAN_POINT('Ctrl Pts',(-78.9530275699163,-4.81776529236232,
-0.409895486782259));
#43928=CARTESIAN_POINT('Ctrl Pts',(-78.8344954706662,-4.04077471622703,
-2.65537500639809));
#43929=CARTESIAN_POINT('Ctrl Pts',(-78.7159633714162,-2.28795537184552,
-4.25959352266151));
#43930=CARTESIAN_POINT('Ctrl Pts',(-78.5974312721659,0.01739479617826,-4.83513950555424));
#43931=CARTESIAN_POINT('Ctrl Pts',(-78.478899172916,2.31854423494792,-4.24302128664049));
#43932=CARTESIAN_POINT('Ctrl Pts',(-78.3603670736658,4.05977569031068,-2.62623257810987));
#43933=CARTESIAN_POINT('Ctrl Pts',(-78.2418349744158,4.82058987944276,-0.375220821371348));
#43934=CARTESIAN_POINT('Ctrl Pts',(-78.1233028751657,4.41725319853946,1.96640547070156));
#43935=CARTESIAN_POINT('Ctrl Pts',(-78.0047707759156,2.94717049047626,3.8331529390692));
#43936=CARTESIAN_POINT('Ctrl Pts',(-77.8862386766655,0.76535831765424,4.77421302627773));
#43937=CARTESIAN_POINT('Ctrl Pts',(-77.7677065774155,-1.60128207237705,
4.56231898362465));
#43938=CARTESIAN_POINT('Ctrl Pts',(-77.6491744781652,-3.58122482847114,
3.24865234734018));
#43939=CARTESIAN_POINT('Ctrl Pts',(-77.5306423789153,-4.69630852858792,
1.15043733326802));
#43940=CARTESIAN_POINT('Ctrl Pts',(-77.4121102796651,-4.67727418140591,
-1.22557573136684));
#43941=CARTESIAN_POINT('Ctrl Pts',(-77.2935781804151,-3.52866076203249,
-3.30567289786488));
#43942=CARTESIAN_POINT('Ctrl Pts',(-77.175046081165,-1.52796948792018,-4.58735411440459));
#43943=CARTESIAN_POINT('Ctrl Pts',(-77.0565139819149,0.841876007549669,
-4.76143359367224));
#43944=CARTESIAN_POINT('Ctrl Pts',(-76.9379818826649,3.00809699385548,-3.78519835053903));
#43945=CARTESIAN_POINT('Ctrl Pts',(-76.8194497834148,4.44851123665998,-1.89576151021052));
#43946=CARTESIAN_POINT('Ctrl Pts',(-76.7009176841646,4.8133511172984,0.453319248329923));
#43947=CARTESIAN_POINT('Ctrl Pts',(-76.5823855849146,4.01836466947884,2.68924789011108));
#43948=CARTESIAN_POINT('Ctrl Pts',(-76.4638534856645,2.24777612232952,4.28313331688481));
#43949=CARTESIAN_POINT('Ctrl Pts',(-76.3453213864143,-0.0552396126277808,
4.82788022852029));
#43950=CARTESIAN_POINT('Ctrl Pts',(-76.1872785874144,-3.1348690121619,4.03636893924357));
#43951=CARTESIAN_POINT('Ctrl Pts',(-75.9897250886641,-5.46268474636236,
0.383518086680876));
#43952=CARTESIAN_POINT('Ctrl Pts',(-75.752660890164,-3.29948284438696,-4.37397660018102));
#43953=CARTESIAN_POINT('Ctrl Pts',(-75.5155966916638,1.85921066417732,-5.14902780119111));
#43954=CARTESIAN_POINT('Ctrl Pts',(-75.2785324931636,5.33003300399772,-1.25678412097787));
#43955=CARTESIAN_POINT('Ctrl Pts',(-75.0414682946635,3.96317201763163,3.77943201826544));
#43956=CARTESIAN_POINT('Ctrl Pts',(-74.8044040961632,-1.00102640242734,
5.38353387637129));
#43957=CARTESIAN_POINT('Ctrl Pts',(-74.5673398976631,-5.05652699721965,
2.10205725116266));
#43958=CARTESIAN_POINT('Ctrl Pts',(-74.330275699163,-4.52254930484235,-3.0877885208858));
#43959=CARTESIAN_POINT('Ctrl Pts',(-74.0932115006627,0.116607261737008,
-5.47480709315744));
#43960=CARTESIAN_POINT('Ctrl Pts',(-73.8561473021626,4.64948979270055,-2.8925309892838));
#43961=CARTESIAN_POINT('Ctrl Pts',(-73.6190831036624,4.96303730879198,2.31497289262041));
#43962=CARTESIAN_POINT('Ctrl Pts',(-73.3820189051621,0.770228935911782,
5.42176221691171));
#43963=CARTESIAN_POINT('Ctrl Pts',(-73.1449547066622,-4.11860453374334,
3.60641765272112));
#43964=CARTESIAN_POINT('Ctrl Pts',(-72.9078905081617,-5.27511038571493,
-1.48036102281075));
#43965=CARTESIAN_POINT('Ctrl Pts',(-72.6708263096619,-1.63184941963692,
-5.22733949850035));
#43966=CARTESIAN_POINT('Ctrl Pts',(-72.4732728109114,2.6178396555861,-4.38937278830862));
#43967=CARTESIAN_POINT('Ctrl Pts',(-72.3152300119115,4.47635368167322,-1.80934701821154));
#43968=CARTESIAN_POINT('Ctrl Pts',(-72.1966979126613,4.80756183098992,0.533926724871739));
#43969=CARTESIAN_POINT('Ctrl Pts',(-72.0781658134113,3.96778601335621,2.76332824391123));
#43970=CARTESIAN_POINT('Ctrl Pts',(-71.9596337141612,2.17480996009685,4.31787551427408));
#43971=CARTESIAN_POINT('Ctrl Pts',(-71.8411016149111,-0.145859952194633,
4.83341378330383));
#43972=CARTESIAN_POINT('Ctrl Pts',(-71.7225695156611,-2.43007031967345,
4.17984836074324));
#43973=CARTESIAN_POINT('Ctrl Pts',(-71.6040374164109,-4.12804290050896,
2.51779008072477));
#43974=CARTESIAN_POINT('Ctrl Pts',(-71.4855053171608,-4.82880743122124,
0.247239396420105));
#43975=CARTESIAN_POINT('Ctrl Pts',(-71.3669732179108,-4.36358801195499,
-2.08279133450973));
#43976=CARTESIAN_POINT('Ctrl Pts',(-71.2484411186607,-2.84450685341156,
-3.90995017899927));
#43977=CARTESIAN_POINT('Ctrl Pts',(-71.1299090194105,-0.638527447948997,
-4.79281780914737));
#43978=CARTESIAN_POINT('Ctrl Pts',(-71.0113769201606,1.72167193322502,-4.51826948070633));
#43979=CARTESIAN_POINT('Ctrl Pts',(-70.8928448209103,3.66608617254502,-3.1525657739581));
#43980=CARTESIAN_POINT('Ctrl Pts',(-70.7743127216604,4.72516179394061,-1.02553858814108));
#43981=CARTESIAN_POINT('Ctrl Pts',(-70.6557806224102,4.64313001864252,1.34915491482993));
#43982=CARTESIAN_POINT('Ctrl Pts',(-70.5372485231601,3.43980453487644,3.39803193879275));
#43983=CARTESIAN_POINT('Ctrl Pts',(-70.41871642391,1.40578130568857,4.62630050592838));
#43984=CARTESIAN_POINT('Ctrl Pts',(-70.30018432466,-0.967731453376396,4.73733807576673));
#43985=CARTESIAN_POINT('Ctrl Pts',(-70.1816522254099,-3.10754159486907,
3.70433020186553));
#43986=CARTESIAN_POINT('Ctrl Pts',(-70.0631201261598,-4.49689447291763,
1.77674328943389));
#43987=CARTESIAN_POINT('Ctrl Pts',(-69.9445880269097,-4.80026777358941,
-0.579919014773209));
#43988=CARTESIAN_POINT('Ctrl Pts',(-69.8260559276597,-3.94439817056713,
-2.79653353348927));
#43989=CARTESIAN_POINT('Ctrl Pts',(-69.7075238284095,-2.13597431478577,
-4.33779788014045));
#43990=CARTESIAN_POINT('Ctrl Pts',(-69.5889917291594,0.188277650519182,
-4.83150372703897));
#43991=CARTESIAN_POINT('Ctrl Pts',(-69.4704596299094,2.46706141544487,-4.15842334294387));
#43992=CARTESIAN_POINT('Ctrl Pts',(-69.3519275306592,4.15006104346198,-2.48110259124925));
#43993=CARTESIAN_POINT('Ctrl Pts',(-69.2333954314092,4.83083975921817,-0.204606820614051));
#43994=CARTESIAN_POINT('Ctrl Pts',(-69.1148633321591,4.34499259254299,2.12130056844982));
#43995=CARTESIAN_POINT('Ctrl Pts',(-68.9963312329089,2.8098494293572,3.93492349548534));
#43996=CARTESIAN_POINT('Ctrl Pts',(-68.877799133659,0.596140378289115,4.79828025235803));
#43997=CARTESIAN_POINT('Ctrl Pts',(-68.7592670344088,-1.76153386927439,
4.50287409976691));
#43998=CARTESIAN_POINT('Ctrl Pts',(-68.6407349351588,-3.6938056800729,3.12004428313488));
#43999=CARTESIAN_POINT('Ctrl Pts',(-68.5222028359086,-4.7340401791978,0.983737928842413));
#44000=CARTESIAN_POINT('Ctrl Pts',(-68.4036707366586,-4.63102545499782,
-1.39013667171659));
#44001=CARTESIAN_POINT('Ctrl Pts',(-68.2851386374085,-3.40963909595999,
-3.42829957357751));
#44002=CARTESIAN_POINT('Ctrl Pts',(-68.1666065381584,-1.36484036594256,
-4.6385436837855));
#44003=CARTESIAN_POINT('Ctrl Pts',(-68.0480744389084,1.00956111970321,-4.72860054101359));
#44004=CARTESIAN_POINT('Ctrl Pts',(-67.9295423396582,3.14015817566407,-3.67672182286094));
#44005=CARTESIAN_POINT('Ctrl Pts',(-67.8110102404082,4.51242128017076,-1.73693146702832));
#44006=CARTESIAN_POINT('Ctrl Pts',(-67.692478141158,4.79495511991091,0.622319957040978));
#44007=CARTESIAN_POINT('Ctrl Pts',(-67.573946041908,3.9195290545396,2.83128393516286));
#44008=CARTESIAN_POINT('Ctrl Pts',(-67.4554139426579,2.09755450673732,4.35650568944393));
#44009=CARTESIAN_POINT('Ctrl Pts',(-67.3368818434078,-0.23096993712172,
4.82965108667669));
#44010=CARTESIAN_POINT('Ctrl Pts',(-67.2183497441577,-2.50371618915523,
4.1364576602515));
#44011=CARTESIAN_POINT('Ctrl Pts',(-67.0998176449076,-4.17182634172216,
2.44432847739504));
#44012=CARTESIAN_POINT('Ctrl Pts',(-66.9812855456576,-4.83245936176243,
0.161905057999808));
#44013=CARTESIAN_POINT('Ctrl Pts',(-66.8627534464075,-4.32607537245367,
-2.15961769828392));
#44014=CARTESIAN_POINT('Ctrl Pts',(-66.7442213471574,-2.77496380957702,
-3.95960257935429));
#44015=CARTESIAN_POINT('Ctrl Pts',(-66.6256892479073,-0.553711077644903,
-4.80336140357819));
#44016=CARTESIAN_POINT('Ctrl Pts',(-66.5071571486572,1.80126036716239,-4.48713024332717));
#44017=CARTESIAN_POINT('Ctrl Pts',(-66.3886250494071,3.72123560623268,-3.08727748895322));
#44018=CARTESIAN_POINT('Ctrl Pts',(-66.270092950157,4.74254933091315,-0.941861229028204));
#44019=CARTESIAN_POINT('Ctrl Pts',(-66.151560850907,4.61855891074222,1.43101024416146));
#44020=CARTESIAN_POINT('Ctrl Pts',(-66.0330287516568,3.37920746960428,3.45829923636778));
#44021=CARTESIAN_POINT('Ctrl Pts',(-65.9144966524068,1.32379275717391,4.6504246544746));
#44022=CARTESIAN_POINT('Ctrl Pts',(-65.7959645531566,-1.05131189961462,
4.71949361908881));
#44023=CARTESIAN_POINT('Ctrl Pts',(-65.6774324539066,-3.17252950280694,
3.64882628864555));
#44024=CARTESIAN_POINT('Ctrl Pts',(-65.5589003546565,-4.52759562591996,
1.69698396546396));
#44025=CARTESIAN_POINT('Ctrl Pts',(-65.4403682554064,-4.78926794861912,
-0.664672285582053));
#44026=CARTESIAN_POINT('Ctrl Pts',(-65.3218361561563,-3.89435379226919,
-2.86581319550488));
#44027=CARTESIAN_POINT('Ctrl Pts',(-65.2033040569063,-2.05897086509784,
-4.37487322188536));
#44028=CARTESIAN_POINT('Ctrl Pts',(-65.0847719576561,0.273644183741452,
-4.82742121547268));
#44029=CARTESIAN_POINT('Ctrl Pts',(-64.9662398584062,2.5401754038242,-4.11416888918016));
#44030=CARTESIAN_POINT('Ctrl Pts',(-64.8477077591559,4.19326578952573,-2.40736344353829));
#44031=CARTESIAN_POINT('Ctrl Pts',(-64.7291756599059,4.83370151333408,-0.119190649311063));
#44032=CARTESIAN_POINT('Ctrl Pts',(-64.6106435606558,4.30682025382488,2.19776614591613));
#44033=CARTESIAN_POINT('Ctrl Pts',(-64.4921114614057,2.73986144452965,3.98397238891927));
#44034=CARTESIAN_POINT('Ctrl Pts',(-64.3735793621556,0.511238528066523,
4.80806737664019));
#44035=CARTESIAN_POINT('Ctrl Pts',(-64.2550472629056,-1.8408461732611,4.47103590874434));
#44036=CARTESIAN_POINT('Ctrl Pts',(-64.1365151636554,-3.74837487629322,
3.0542695555018));
#44037=CARTESIAN_POINT('Ctrl Pts',(-64.0179830644054,-4.75068805435598,
0.899910962868411));
#44038=CARTESIAN_POINT('Ctrl Pts',(-63.8994509651552,-4.60573162278402,
-1.47177204409466));
#44039=CARTESIAN_POINT('Ctrl Pts',(-63.7809188659052,-3.34851190208522,
-3.48802878034068));
#44040=CARTESIAN_POINT('Ctrl Pts',(-63.6623867666551,-1.28264175037359,
-4.66194239251087));
#44041=CARTESIAN_POINT('Ctrl Pts',(-63.5438546674051,1.09298056427011,-4.71001806971258));
#44042=CARTESIAN_POINT('Ctrl Pts',(-63.4253225681549,3.20465303186822,-3.62064575403741));
#44043=CARTESIAN_POINT('Ctrl Pts',(-63.3067904689049,4.54241633287416,-1.65690391686706));
#44044=CARTESIAN_POINT('Ctrl Pts',(-63.1882583696547,4.78320669998339,0.706972698288407));
#44045=CARTESIAN_POINT('Ctrl Pts',(-63.0697262704047,3.86887435208713,2.90011861458352));
#44046=CARTESIAN_POINT('Ctrl Pts',(-62.9511941711546,2.02022640256444,4.39289904428418));
#44047=CARTESIAN_POINT('Ctrl Pts',(-62.8326620719045,-0.316297056721141,
4.82481428687165));
#44048=CARTESIAN_POINT('Ctrl Pts',(-62.7141299726544,-2.57643621195637,
4.09155877100791));
#44049=CARTESIAN_POINT('Ctrl Pts',(-62.5955978734043,-4.21437771217373,
2.37021037674359));
#44050=CARTESIAN_POINT('Ctrl Pts',(-62.4770657741542,-4.8345661169712,0.0764669309488382));
#44051=CARTESIAN_POINT('Ctrl Pts',(-62.3585336749042,-4.28722874059428,
-2.23574293171377));
#44052=CARTESIAN_POINT('Ctrl Pts',(-62.2400015756541,-2.70454507598614,
-4.00803102069538));
#44053=CARTESIAN_POINT('Ctrl Pts',(-62.121469476404,-0.468726046964763,
-4.81239780398398));
#44054=CARTESIAN_POINT('Ctrl Pts',(-62.0029373771539,1.8802881956162,-4.45459235309891));
#44055=CARTESIAN_POINT('Ctrl Pts',(-61.8844052779038,3.77522137048981,-3.02102306094952));
#44056=CARTESIAN_POINT('Ctrl Pts',(-61.7658731786537,4.75845571380694,-0.857890406984954));
#44057=CARTESIAN_POINT('Ctrl Pts',(-61.6473410794037,4.59254459307791,1.5124188877089));
#44058=CARTESIAN_POINT('Ctrl Pts',(-61.5288089801535,3.31755479085771,3.517485883414));
#44059=CARTESIAN_POINT('Ctrl Pts',(-61.4102768809035,1.24139055993465,4.67309599824245));
#44060=CARTESIAN_POINT('Ctrl Pts',(-61.2917447816533,-1.13456385942904,
4.70017463305793));
#44061=CARTESIAN_POINT('Ctrl Pts',(-61.1732126824033,-3.23652625297439,
3.59218242001983));
#44062=CARTESIAN_POINT('Ctrl Pts',(-61.0546805831532,-4.55688224501281,
1.61669445203919));
#44063=CARTESIAN_POINT('Ctrl Pts',(-60.9361484839031,-4.77677184423655,
-0.749217891692864));
#44064=CARTESIAN_POINT('Ctrl Pts',(-60.817616384653,-3.84309273056335,-2.93419751186658));
#44065=CARTESIAN_POINT('Ctrl Pts',(-60.699084285403,-1.9813241324019,-4.41058175075367));
#44066=CARTESIAN_POINT('Ctrl Pts',(-60.5805521861528,0.358925198440316,
-4.82183050033724));
#44067=CARTESIAN_POINT('Ctrl Pts',(-60.4620200869028,2.6124958339146,-4.06862908012547));
#44068=CARTESIAN_POINT('Ctrl Pts',(-60.3434879876527,4.23516035471804,-2.33287216207629));
#44069=CARTESIAN_POINT('Ctrl Pts',(-60.2249558884025,4.83505331855051,-0.0337372739214764));
#44070=CARTESIAN_POINT('Ctrl Pts',(-60.1064237891525,4.26730193315002,2.27354515783043));
#44071=CARTESIAN_POINT('Ctrl Pts',(-59.9878916899025,2.66901832824221,4.03177645770732));
#44072=CARTESIAN_POINT('Ctrl Pts',(-59.8693595906523,0.426175210907464,
4.81635262496778));
#44073=CARTESIAN_POINT('Ctrl Pts',(-59.7508274914023,-1.91957984074924,
4.43780030160997));
#44074=CARTESIAN_POINT('Ctrl Pts',(-59.6322953921521,-3.80178006744974,
2.98754172835162));
#44075=CARTESIAN_POINT('Ctrl Pts',(-59.5137632929021,-4.76583745049515,
0.815800574795077));
#44076=CARTESIAN_POINT('Ctrl Pts',(-59.395231193652,-4.57902756281045,-1.55294302820165));
#44077=CARTESIAN_POINT('Ctrl Pts',(-59.2766990944019,-3.28628066519173,
-3.54667748409246));
#44078=CARTESIAN_POINT('Ctrl Pts',(-59.1581669951518,-1.20015991556334,
-4.68386547959001));
#44079=CARTESIAN_POINT('Ctrl Pts',(-59.0396348959018,1.17630498730679,-4.69000696058032));
#44080=CARTESIAN_POINT('Ctrl Pts',(-58.9606134964017,2.57036993835409,-3.93879461861823));
#44081=CARTESIAN_POINT('Ctrl Pts',(-58.9211027966516,3.13634117333409,-3.41972378108142));
#44082=CARTESIAN_POINT('Ctrl Pts',(-89.575,-2.1683958723107,4.42195480991675));
#44083=CARTESIAN_POINT('Ctrl Pts',(-89.53548930025,-2.90023837919381,4.0630808866582));
#44084=CARTESIAN_POINT('Ctrl Pts',(-89.4564679007499,-4.18158777943873,
2.97533030318424));
#44085=CARTESIAN_POINT('Ctrl Pts',(-89.3379358014998,-5.09393729919481,
0.623762189627529));
#44086=CARTESIAN_POINT('Ctrl Pts',(-89.2194037022498,-4.7760113611239,-1.87790340886064));
#44087=CARTESIAN_POINT('Ctrl Pts',(-89.1008716029996,-3.30475671773202,
-3.92632446201307));
#44088=CARTESIAN_POINT('Ctrl Pts',(-88.9823395037497,-1.035390253221,-5.02642719512737));
#44089=CARTESIAN_POINT('Ctrl Pts',(-88.8638074044994,1.48400432002415,-4.91273446231162));
#44090=CARTESIAN_POINT('Ctrl Pts',(-88.7452753052495,3.6450255042766,-3.61260692861675));
#44091=CARTESIAN_POINT('Ctrl Pts',(-88.6267432059992,4.92578613196527,-1.44006696053689));
#44092=CARTESIAN_POINT('Ctrl Pts',(-88.5082111067493,5.01699346462279,1.08025046241909));
#44093=CARTESIAN_POINT('Ctrl Pts',(-88.3896790074991,3.89661879247731,3.33968841879312));
#44094=CARTESIAN_POINT('Ctrl Pts',(-88.2711469082491,1.83522878269921,4.79260870230941));
#44095=CARTESIAN_POINT('Ctrl Pts',(-88.1526148089989,-0.669360859787416,
5.08813477323801));
#44096=CARTESIAN_POINT('Ctrl Pts',(-88.0340827097489,-3.01230278811849,
4.15489985799353));
#44097=CARTESIAN_POINT('Ctrl Pts',(-87.9155506104988,-4.62778731241589,
2.21827524343903));
#44098=CARTESIAN_POINT('Ctrl Pts',(-87.7970185112487,-5.12568217307047,
-0.254052660266212));
#44099=CARTESIAN_POINT('Ctrl Pts',(-87.6784864119986,-4.38574805857882,
-2.66502805736134));
#44100=CARTESIAN_POINT('Ctrl Pts',(-87.5599543127485,-2.58667568127932,
-4.43241124189013));
#44101=CARTESIAN_POINT('Ctrl Pts',(-87.4414222134984,-0.162932866706595,
-5.1293872371898));
#44102=CARTESIAN_POINT('Ctrl Pts',(-87.3228901142484,2.30015749744563,-4.5876394813756));
#44103=CARTESIAN_POINT('Ctrl Pts',(-87.2043580149983,4.20777026179349,-2.93799761002543));
#44104=CARTESIAN_POINT('Ctrl Pts',(-87.0858259157481,5.09922560038977,-0.578842644798489));
#44105=CARTESIAN_POINT('Ctrl Pts',(-86.9672938164982,4.75924109322802,1.92010019187045));
#44106=CARTESIAN_POINT('Ctrl Pts',(-86.8487617172479,3.2699214564463,3.95534754478431));
#44107=CARTESIAN_POINT('Ctrl Pts',(-86.730229617998,0.990930624635091,5.03539641217931));
#44108=CARTESIAN_POINT('Ctrl Pts',(-86.6116975187478,-1.52736545681198,
4.89941989345072));
#44109=CARTESIAN_POINT('Ctrl Pts',(-86.4931654194978,-3.6768097106286,3.58025570074025));
#44110=CARTESIAN_POINT('Ctrl Pts',(-86.3746333202476,-4.93832110226258,
1.39647600116869));
#44111=CARTESIAN_POINT('Ctrl Pts',(-86.2561012209977,-5.0072503545504,-1.12454631641016));
#44112=CARTESIAN_POINT('Ctrl Pts',(-86.1375691217474,-3.86695136581583,
-3.37399580101973));
#44113=CARTESIAN_POINT('Ctrl Pts',(-86.0190370224974,-1.79280116791488,
-4.80864060865615));
#44114=CARTESIAN_POINT('Ctrl Pts',(-85.9005049232473,0.71430237748739,-5.08202052774328));
#44115=CARTESIAN_POINT('Ctrl Pts',(-85.7819728239972,3.04890513975984,-4.12811554824192));
#44116=CARTESIAN_POINT('Ctrl Pts',(-85.6634407247472,4.64721114470303,-2.17728939450819));
#44117=CARTESIAN_POINT('Ctrl Pts',(-85.544908625497,5.12323674418264,0.299342268894373));
#44118=CARTESIAN_POINT('Ctrl Pts',(-85.426376526247,4.36202391581492,2.70368413257703));
#44119=CARTESIAN_POINT('Ctrl Pts',(-85.3078444269969,2.54740210376838,4.45509854577948));
#44120=CARTESIAN_POINT('Ctrl Pts',(-85.1893123277468,0.117594242094089,
5.13062687447805));
#44121=CARTESIAN_POINT('Ctrl Pts',(-85.0707802284967,-2.34061209548073,
4.56713209239445));
#44122=CARTESIAN_POINT('Ctrl Pts',(-84.9522481292467,-4.23357123215246,
2.90069563263386));
#44123=CARTESIAN_POINT('Ctrl Pts',(-84.8337160299965,-5.10414212541622,
0.533754339037759));
#44124=CARTESIAN_POINT('Ctrl Pts',(-84.7151839307465,-4.74208585462591,
-1.96208620561045));
#44125=CARTESIAN_POINT('Ctrl Pts',(-84.5966518314963,-3.23483736640461,
-3.98409183425815));
#44126=CARTESIAN_POINT('Ctrl Pts',(-84.4781197322463,-0.946390331757192,
-5.04395736211623));
#44127=CARTESIAN_POINT('Ctrl Pts',(-84.3595876329962,1.57060567391381,-4.88573007317839));
#44128=CARTESIAN_POINT('Ctrl Pts',(-84.2410555337461,3.70830753570835,-3.54762113979195));
#44129=CARTESIAN_POINT('Ctrl Pts',(-84.122523434496,4.95046995348558,-1.35277779791302));
#44130=CARTESIAN_POINT('Ctrl Pts',(-84.0039913352459,4.99711633946695,1.16875524414756));
#44131=CARTESIAN_POINT('Ctrl Pts',(-83.885459235996,3.83698180308851,3.40803919778774));
#44132=CARTESIAN_POINT('Ctrl Pts',(-83.7669271367456,1.7502335709595,4.82429714859857));
#44133=CARTESIAN_POINT('Ctrl Pts',(-83.6483950374958,-0.759188127149455,
5.0755092275047));
#44134=CARTESIAN_POINT('Ctrl Pts',(-83.5298629382456,-3.08526933724734,
4.10100885728516));
#44135=CARTESIAN_POINT('Ctrl Pts',(-83.4113308389955,-4.66627200131942,
2.13613345570741));
#44136=CARTESIAN_POINT('Ctrl Pts',(-83.2927987397455,-5.12039114954072,
-0.344608483057541));
#44137=CARTESIAN_POINT('Ctrl Pts',(-83.1742666404952,-4.33795906810922,
-2.74212903677033));
#44138=CARTESIAN_POINT('Ctrl Pts',(-83.0557345412453,-2.50792955452944,
-4.47743787007791));
#44139=CARTESIAN_POINT('Ctrl Pts',(-82.9372024419952,-0.0722464328626828,
-5.13146577342465));
#44140=CARTESIAN_POINT('Ctrl Pts',(-82.818670342745,2.38088387453369,-4.54626797570001));
#44141=CARTESIAN_POINT('Ctrl Pts',(-82.7001382434951,4.25904152911249,-2.86316708981246));
#44142=CARTESIAN_POINT('Ctrl Pts',(-82.5816061442448,5.1086599791349,-0.488624342900971));
#44143=CARTESIAN_POINT('Ctrl Pts',(-82.4630740449948,4.72456022392924,2.00391896576577));
#44144=CARTESIAN_POINT('Ctrl Pts',(-82.3445419457448,3.19950061158604,4.01252493666403));
#44145=CARTESIAN_POINT('Ctrl Pts',(-82.2260098464945,0.901776118770504,
5.05212434155229));
#44146=CARTESIAN_POINT('Ctrl Pts',(-82.1074777472446,-1.61372321506223,
4.87165864116722));
#44147=CARTESIAN_POINT('Ctrl Pts',(-81.9889456479944,-3.73951571447014,
3.51470948331734));
#44148=CARTESIAN_POINT('Ctrl Pts',(-81.8704135487444,-4.96223213629194,
1.30897393268221));
#44149=CARTESIAN_POINT('Ctrl Pts',(-81.7518814494944,-4.98659201253917,
-1.21287288343444));
#44150=CARTESIAN_POINT('Ctrl Pts',(-81.6333493502442,-3.80671254362719,
-3.44181640141966));
#44151=CARTESIAN_POINT('Ctrl Pts',(-81.5148172509941,-1.70752926778261,
-4.83957687515715));
#44152=CARTESIAN_POINT('Ctrl Pts',(-81.3962851517441,0.804014578588726,
-5.06860149235535));
#44153=CARTESIAN_POINT('Ctrl Pts',(-81.2777530524939,3.12139255231928,-4.0735818471237));
#44154=CARTESIAN_POINT('Ctrl Pts',(-81.1592209532439,4.68496838748752,-2.09481066904211));
#44155=CARTESIAN_POINT('Ctrl Pts',(-81.0406888539937,5.11714561437722,0.389847780742552));
#44156=CARTESIAN_POINT('Ctrl Pts',(-80.9221567547437,4.31355539363008,2.78035976035025));
#44157=CARTESIAN_POINT('Ctrl Pts',(-80.8036246554936,2.46826111739352,4.49942747327406));
#44158=CARTESIAN_POINT('Ctrl Pts',(-80.6850925562435,0.0268929806491242,
5.13190386683944));
#44159=CARTESIAN_POINT('Ctrl Pts',(-80.5665604569934,-2.42096968889947,
4.52504876176164));
#44160=CARTESIAN_POINT('Ctrl Pts',(-80.4480283577434,-4.28417916334405,
2.82541491240804));
#44161=CARTESIAN_POINT('Ctrl Pts',(-80.3294962584932,-5.11277880862357,
0.443456181579524));
#44162=CARTESIAN_POINT('Ctrl Pts',(-80.2109641592432,-4.70666557004154,
-2.04559520498919));
#44163=CARTESIAN_POINT('Ctrl Pts',(-80.0924320599931,-3.16391395204272,
-4.04064463111481));
#44164=CARTESIAN_POINT('Ctrl Pts',(-79.9738999607429,-0.857091470380425,
-5.05989671261218));
#44165=CARTESIAN_POINT('Ctrl Pts',(-79.855367861493,1.65671471245823,-4.85720669648522));
#44166=CARTESIAN_POINT('Ctrl Pts',(-79.7368357622428,3.77043180932637,-3.48152330197269));
#44167=CARTESIAN_POINT('Ctrl Pts',(-79.6183036629927,4.97360673196066,-1.26506782686858));
#44168=CARTESIAN_POINT('Ctrl Pts',(-79.4997715637427,4.9756781958107,1.25689578833165));
#44169=CARTESIAN_POINT('Ctrl Pts',(-79.3812394644924,3.77614595165346,3.47532477371217));
#44170=CARTESIAN_POINT('Ctrl Pts',(-79.2627073652425,1.66469159397173,4.85447859477892));
#44171=CARTESIAN_POINT('Ctrl Pts',(-79.1441752659923,-0.848778230657501,
5.06129786202729));
#44172=CARTESIAN_POINT('Ctrl Pts',(-79.0256431667423,-3.15727196322148,
4.04583665963461));
#44173=CARTESIAN_POINT('Ctrl Pts',(-78.9071110674922,-4.70329884341097,
2.05332426288532));
#44174=CARTESIAN_POINT('Ctrl Pts',(-78.7885789682421,-5.11350039112483,
-0.435056629949174));
#44175=CARTESIAN_POINT('Ctrl Pts',(-78.670046868992,-4.28881480063609,-2.81837331414327));
#44176=CARTESIAN_POINT('Ctrl Pts',(-78.551514769742,-2.42839988642778,-4.52106564400155));
#44177=CARTESIAN_POINT('Ctrl Pts',(-78.4329826704918,0.0184625633801521,
-5.13194110804669));
#44178=CARTESIAN_POINT('Ctrl Pts',(-78.3144505712419,2.46086642515392,-4.50347613304934));
#44179=CARTESIAN_POINT('Ctrl Pts',(-78.1959184719916,4.30898213601093,-2.78744199860449));
#44180=CARTESIAN_POINT('Ctrl Pts',(-78.0773863727416,5.11649836347594,-0.398253484843363));
#44181=CARTESIAN_POINT('Ctrl Pts',(-77.9588542734915,4.68840314704361,2.08711187310909));
#44182=CARTESIAN_POINT('Ctrl Pts',(-77.8403221742414,3.12808045664934,4.06844830823227));
#44183=CARTESIAN_POINT('Ctrl Pts',(-77.7217900749914,0.812339294087262,
5.06727470013674));
#44184=CARTESIAN_POINT('Ctrl Pts',(-77.6032579757413,-1.69957563445067,
4.84237369225633));
#44185=CARTESIAN_POINT('Ctrl Pts',(-77.4847258764911,-3.80105576959598,
3.44806856305101));
#44186=CARTESIAN_POINT('Ctrl Pts',(-77.3661937772411,-4.98458809021849,
1.22105611142095));
#44187=CARTESIAN_POINT('Ctrl Pts',(-77.247661677991,-4.96438533316134,-1.30080682669047));
#44188=CARTESIAN_POINT('Ctrl Pts',(-77.1291295787408,-3.74526509529329,
-3.50858927954838));
#44189=CARTESIAN_POINT('Ctrl Pts',(-77.0105974794909,-1.62176280909601,
-4.86894558674816));
#44190=CARTESIAN_POINT('Ctrl Pts',(-76.8920653802408,0.89355396800014,-5.05371081114237));
#44191=CARTESIAN_POINT('Ctrl Pts',(-76.7735332809906,3.19274689014148,-4.01755006136377));
#44192=CARTESIAN_POINT('Ctrl Pts',(-76.6550011817407,4.72157993762085,-2.01213148330597));
#44193=CARTESIAN_POINT('Ctrl Pts',(-76.5364690824904,5.10881525506152,0.481145928240669));
#44194=CARTESIAN_POINT('Ctrl Pts',(-76.4179369832404,4.26502912909379,2.85432546075147));
#44195=CARTESIAN_POINT('Ctrl Pts',(-76.2994048839903,2.38575426223333,4.54605041176487));
#44196=CARTESIAN_POINT('Ctrl Pts',(-76.1808727847402,-0.0586304569932881,
5.12423622545075));
#44197=CARTESIAN_POINT('Ctrl Pts',(-76.0228299857401,-3.32730071870205,
4.28413857816343));
#44198=CARTESIAN_POINT('Ctrl Pts',(-75.8252764869899,-5.79800776750144,
0.407060071887531));
#44199=CARTESIAN_POINT('Ctrl Pts',(-75.5882122884898,-3.50201925403669,
-4.6424700454491));
#44200=CARTESIAN_POINT('Ctrl Pts',(-75.3511480899896,1.97333698956357,-5.46509721364885));
#44201=CARTESIAN_POINT('Ctrl Pts',(-75.1140838914894,5.65721329219971,-1.33393092111982));
#44202=CARTESIAN_POINT('Ctrl Pts',(-74.8770196929893,4.2064485155352,4.01142976688134));
#44203=CARTESIAN_POINT('Ctrl Pts',(-74.6399554944891,-1.06247369676832,
5.71399827760396));
#44204=CARTESIAN_POINT('Ctrl Pts',(-74.4028912959888,-5.36691831356058,
2.23109054171393));
#44205=CARTESIAN_POINT('Ctrl Pts',(-74.1658270974888,-4.80016278000401,
-3.27733022492635));
#44206=CARTESIAN_POINT('Ctrl Pts',(-73.9287628989886,0.123765115632612,
-5.81087423593989));
#44207=CARTESIAN_POINT('Ctrl Pts',(-73.6916987004883,4.93489541950005,-3.07008694850533));
#44208=CARTESIAN_POINT('Ctrl Pts',(-73.4546345019883,5.26768982704656,2.45707585851558));
#44209=CARTESIAN_POINT('Ctrl Pts',(-73.217570303488,0.817508891785283,5.75457323766176));
#44210=CARTESIAN_POINT('Ctrl Pts',(-72.9805061049879,-4.37142214619141,
3.82779503745949));
#44211=CARTESIAN_POINT('Ctrl Pts',(-72.7434419064876,-5.59891928802401,
-1.57123193218838));
#44212=CARTESIAN_POINT('Ctrl Pts',(-72.5063777079877,-1.73201933659968,
-5.54821601884577));
#44213=CARTESIAN_POINT('Ctrl Pts',(-72.3088242092372,2.77853388249591,-4.65881131764377));
#44214=CARTESIAN_POINT('Ctrl Pts',(-72.1507814102373,4.75113147133521,-1.92041249912545));
#44215=CARTESIAN_POINT('Ctrl Pts',(-72.0322493109871,5.1026705975271,0.566701437446899));
#44216=CARTESIAN_POINT('Ctrl Pts',(-71.9137172117371,4.21134573810842,2.93295318442499));
#44217=CARTESIAN_POINT('Ctrl Pts',(-71.795185112487,2.30830912398487,4.5829252342516));
#44218=CARTESIAN_POINT('Ctrl Pts',(-71.6766530132369,-0.154813461705778,
5.13010945356231));
#44219=CARTESIAN_POINT('Ctrl Pts',(-71.5581209139868,-2.57923845933515,
4.43642538198926));
#44220=CARTESIAN_POINT('Ctrl Pts',(-71.4395888147368,-4.38143988039363,
2.67234283558125));
#44221=CARTESIAN_POINT('Ctrl Pts',(-71.3210567154866,-5.1252203438306,0.262416011070538));
#44222=CARTESIAN_POINT('Ctrl Pts',(-71.2025246162366,-4.63144376111743,
-2.21064200045838));
#44223=CARTESIAN_POINT('Ctrl Pts',(-71.0839925169864,-3.01911488518057,
-4.14995969216005));
#44224=CARTESIAN_POINT('Ctrl Pts',(-70.9654604177364,-0.677723001576583,
-5.08702152438147));
#44225=CARTESIAN_POINT('Ctrl Pts',(-70.8469283184864,1.82735554135264,-4.79562024190483));
#44226=CARTESIAN_POINT('Ctrl Pts',(-70.7283962192361,3.89112626696975,-3.34608378364507));
#44227=CARTESIAN_POINT('Ctrl Pts',(-70.6098641199861,5.01521249276049,-1.08849054558277));
#44228=CARTESIAN_POINT('Ctrl Pts',(-70.4913320207361,4.92814525523101,1.43197183050982));
#44229=CARTESIAN_POINT('Ctrl Pts',(-70.3727999214859,3.65095449177829,3.60661771456934));
#44230=CARTESIAN_POINT('Ctrl Pts',(-70.2542678222359,1.49207419213024,4.91028267483867));
#44231=CARTESIAN_POINT('Ctrl Pts',(-70.1357357229858,-1.02713496093071,
5.02813620699353));
#44232=CARTESIAN_POINT('Ctrl Pts',(-70.0172036237357,-3.29829582731872,
3.9317178788523));
#44233=CARTESIAN_POINT('Ctrl Pts',(-69.8986715244855,-4.77293314445299,
1.88580741362638));
#44234=CARTESIAN_POINT('Ctrl Pts',(-69.7801394252356,-5.09492879959653,
-0.61551693137989));
#44235=CARTESIAN_POINT('Ctrl Pts',(-69.6616073259854,-4.18652224921013,
-2.96819675710668));
#44236=CARTESIAN_POINT('Ctrl Pts',(-69.5430752267354,-2.26708958018463,
-4.60407052038899));
#44237=CARTESIAN_POINT('Ctrl Pts',(-69.4245431274853,0.199834940298159,
-5.12808214985099));
#44238=CARTESIAN_POINT('Ctrl Pts',(-69.3060110282352,2.61850022723304,-4.41368520469782));
#44239=CARTESIAN_POINT('Ctrl Pts',(-69.1874789289851,4.4048095914048,-2.63340331063596));
#44240=CARTESIAN_POINT('Ctrl Pts',(-69.068946829735,5.12737742483736,-0.217166464895158));
#44241=CARTESIAN_POINT('Ctrl Pts',(-68.950414730485,4.61170687509952,2.25151509635759));
#44242=CARTESIAN_POINT('Ctrl Pts',(-68.8318826312348,2.98233003977967,4.17646597793152));
#44243=CARTESIAN_POINT('Ctrl Pts',(-68.7133505319847,0.632734031767687,
5.09281927578678));
#44244=CARTESIAN_POINT('Ctrl Pts',(-68.5948184327347,-1.8696643740188,4.77927982644706));
#44245=CARTESIAN_POINT('Ctrl Pts',(-68.4762863334846,-3.92054731676857,
3.31156598421883));
#44246=CARTESIAN_POINT('Ctrl Pts',(-68.3577542342345,-5.02463587138733,
1.04412398251837));
#44247=CARTESIAN_POINT('Ctrl Pts',(-68.2392221349844,-4.915297661549,-1.47546922341958));
#44248=CARTESIAN_POINT('Ctrl Pts',(-68.1206900357343,-3.61893736883079,
-3.6387433066059));
#44249=CARTESIAN_POINT('Ctrl Pts',(-68.0021579364842,-1.4486201218923,-4.92327739146802));
#44250=CARTESIAN_POINT('Ctrl Pts',(-67.8836258372342,1.07153231159905,-5.01886232487884));
#44251=CARTESIAN_POINT('Ctrl Pts',(-67.765093737984,3.33291455374709,-3.9024147791222));
#44252=CARTESIAN_POINT('Ctrl Pts',(-67.646561638734,4.78941305373535,-1.84355177079443));
#44253=CARTESIAN_POINT('Ctrl Pts',(-67.5280295394838,5.08929003244738,0.660520625356854));
#44254=CARTESIAN_POINT('Ctrl Pts',(-67.4094974402338,4.16012656016829,3.00508028749189));
#44255=CARTESIAN_POINT('Ctrl Pts',(-67.2909653409837,2.22631139952188,4.62392669527201));
#44256=CARTESIAN_POINT('Ctrl Pts',(-67.1724332417336,-0.24514786257484,
5.12611578647664));
#44257=CARTESIAN_POINT('Ctrl Pts',(-67.0539011424836,-2.65740502817917,
4.39037117418312));
#44258=CARTESIAN_POINT('Ctrl Pts',(-66.9353690432334,-4.42791093703134,
2.59437184393606));
#44259=CARTESIAN_POINT('Ctrl Pts',(-66.8168369439834,-5.12909644553283,
0.171843484928528));
#44260=CARTESIAN_POINT('Ctrl Pts',(-66.6983048447333,-4.59162843489841,
-2.29218429597677));
#44261=CARTESIAN_POINT('Ctrl Pts',(-66.5797727454832,-2.94530299102049,
-4.20265996982576));
#44262=CARTESIAN_POINT('Ctrl Pts',(-66.4612406462331,-0.587700238655496,
-5.0982123298637));
#44263=CARTESIAN_POINT('Ctrl Pts',(-66.342708546983,1.91182945474832,-4.76256954456801));
#44264=CARTESIAN_POINT('Ctrl Pts',(-66.2241764477329,3.9496610094528,-3.2767878236618));
#44265=CARTESIAN_POINT('Ctrl Pts',(-66.1056443484829,5.03366735133376,-0.999676711245437));
#44266=CARTESIAN_POINT('Ctrl Pts',(-65.9871122492328,4.90206586733353,1.51885179106248));
#44267=CARTESIAN_POINT('Ctrl Pts',(-65.8685801499827,3.58663771871725,3.67058447737751));
#44268=CARTESIAN_POINT('Ctrl Pts',(-65.7500480507326,1.40505283482956,4.93588766709976));
#44269=CARTESIAN_POINT('Ctrl Pts',(-65.6315159514825,-1.11584593346544,
5.00919638102347));
#44270=CARTESIAN_POINT('Ctrl Pts',(-65.5129838522324,-3.36727297180218,
3.87280689736275));
#44271=CARTESIAN_POINT('Ctrl Pts',(-65.3944517529823,-4.80551886591482,
1.80115212023493));
#44272=CARTESIAN_POINT('Ctrl Pts',(-65.2759196537322,-5.08325375818739,
-0.705472721488053));
#44273=CARTESIAN_POINT('Ctrl Pts',(-65.1573875544821,-4.13340593231403,
-3.04172910194205));
#44274=CARTESIAN_POINT('Ctrl Pts',(-65.0388554552321,-2.18535932845954,
-4.6434217056396));
#44275=CARTESIAN_POINT('Ctrl Pts',(-64.9203233559819,0.290441637497185,
-5.12374903621342));
#44276=CARTESIAN_POINT('Ctrl Pts',(-64.8017912567319,2.69610226583112,-4.36671422273892));
#44277=CARTESIAN_POINT('Ctrl Pts',(-64.6832591574818,4.45066643010254,-2.55513773774495));
#44278=CARTESIAN_POINT('Ctrl Pts',(-64.5647270582317,5.13041484569598,-0.126507082617098));
#44279=CARTESIAN_POINT('Ctrl Pts',(-64.4461949589817,4.57119135449609,2.33267445895697));
#44280=CARTESIAN_POINT('Ctrl Pts',(-64.3276628597315,2.90804589223992,4.22852570283266));
#44281=CARTESIAN_POINT('Ctrl Pts',(-64.2091307604815,0.54262054180405,5.10320717573785));
#44282=CARTESIAN_POINT('Ctrl Pts',(-64.0905986612314,-1.95384520742303,
4.74548727069414));
#44283=CARTESIAN_POINT('Ctrl Pts',(-63.9720665619812,-3.97846620431968,
3.24175372167231));
#44284=CARTESIAN_POINT('Ctrl Pts',(-63.8535344627312,-5.04230566453141,
0.955151357809071));
#44285=CARTESIAN_POINT('Ctrl Pts',(-63.7350023634811,-4.88845118541963,
-1.5621157251175));
#44286=CARTESIAN_POINT('Ctrl Pts',(-63.616470264231,-3.55405792559961,-3.70213894828012));
#44287=CARTESIAN_POINT('Ctrl Pts',(-63.4979381649809,-1.36137580272046,
-4.94811241330038));
#44288=CARTESIAN_POINT('Ctrl Pts',(-63.3794060657308,1.16007239948927,-4.99913918178251));
#44289=CARTESIAN_POINT('Ctrl Pts',(-63.2608739664808,3.40136838086655,-3.84289652066398));
#44290=CARTESIAN_POINT('Ctrl Pts',(-63.1423418672306,4.82124933143318,-1.7586117863375));
#44291=CARTESIAN_POINT('Ctrl Pts',(-63.0238097679807,5.07682044411155,0.750369714967913));
#44292=CARTESIAN_POINT('Ctrl Pts',(-62.9052776687304,4.10636245480316,3.07814033479194));
#44293=CARTESIAN_POINT('Ctrl Pts',(-62.7867455694805,2.14423656462699,4.66255403033645));
#44294=CARTESIAN_POINT('Ctrl Pts',(-62.6682134702303,-0.335712726773787,
5.12098208315281));
#44295=CARTESIAN_POINT('Ctrl Pts',(-62.5496813709803,-2.73458891790202,
4.34271619853037));
#44296=CARTESIAN_POINT('Ctrl Pts',(-62.4311492717301,-4.47307429311926,
2.51570405634761));
#44297=CARTESIAN_POINT('Ctrl Pts',(-62.3126171724801,-5.13133252241295,
0.0811607991645035));
#44298=CARTESIAN_POINT('Ctrl Pts',(-62.19408507323,-4.55039723014839,-2.37298242276288));
#44299=CARTESIAN_POINT('Ctrl Pts',(-62.0755529739799,-2.87056165351069,
-4.25406115662326));
#44300=CARTESIAN_POINT('Ctrl Pts',(-61.9570208747298,-0.497498462261037,
-5.10780342328676));
#44301=CARTESIAN_POINT('Ctrl Pts',(-61.8384887754797,1.99570835029122,-4.72803433907091));
#44302=CARTESIAN_POINT('Ctrl Pts',(-61.7199566762297,4.00696065148427,-3.20646641467831));
#44303=CARTESIAN_POINT('Ctrl Pts',(-61.6014245769795,5.05055013623774,-0.910551399964303));
#44304=CARTESIAN_POINT('Ctrl Pts',(-61.4828924777295,4.87445467926628,1.60525764634163));
#44305=CARTESIAN_POINT('Ctrl Pts',(-61.3643603784793,3.52120053409885,3.73340425469211));
#44306=CARTESIAN_POINT('Ctrl Pts',(-61.2458282792294,1.31759243727128,4.95995067519358));
#44307=CARTESIAN_POINT('Ctrl Pts',(-61.1272961799792,-1.20420825567067,
4.98869151276398));
#44308=CARTESIAN_POINT('Ctrl Pts',(-61.0087640807292,-3.43519811699984,
3.81268598511499));
#44309=CARTESIAN_POINT('Ctrl Pts',(-60.890231981479,-4.83660322330837,1.71593409208573));
#44310=CARTESIAN_POINT('Ctrl Pts',(-60.771699882229,-5.06999058931756,-0.795208099548269));
#44311=CARTESIAN_POINT('Ctrl Pts',(-60.6531677829788,-4.07899824676367,
-3.11431114096681));
#44312=CARTESIAN_POINT('Ctrl Pts',(-60.5346356837288,-2.10294630625613,
-4.68132217717649));
#44313=CARTESIAN_POINT('Ctrl Pts',(-60.4161035844787,0.38095756667902,-5.11781513900239));
#44314=CARTESIAN_POINT('Ctrl Pts',(-60.2975714852286,2.77286203412865,-4.31837898486793));
#44315=CARTESIAN_POINT('Ctrl Pts',(-60.1790393859785,4.49513266340712,-2.47607386190709));
#44316=CARTESIAN_POINT('Ctrl Pts',(-60.0605072867284,5.13184963051497,-0.0358082125060307));
#44317=CARTESIAN_POINT('Ctrl Pts',(-59.9419751874783,4.52924722979,2.41310511166584));
#44318=CARTESIAN_POINT('Ctrl Pts',(-59.8234430882283,2.83285412160331,4.27926419041165));
#44319=CARTESIAN_POINT('Ctrl Pts',(-59.7049109889781,0.452335673370796,
5.11200100814619));
#44320=CARTESIAN_POINT('Ctrl Pts',(-59.5863788897281,-2.03741188513844,
4.71021151943447));
#44321=CARTESIAN_POINT('Ctrl Pts',(-59.467846790478,-4.03514963518333,3.17092985427215));
#44322=CARTESIAN_POINT('Ctrl Pts',(-59.3493146912279,-5.05838499558678,
0.865877913336275));
#44323=CARTESIAN_POINT('Ctrl Pts',(-59.2307825919778,-4.86010791570163,
-1.64826933240034));
#44324=CARTESIAN_POINT('Ctrl Pts',(-59.1122504927277,-3.48800666845358,
-3.76438776103343));
#44325=CARTESIAN_POINT('Ctrl Pts',(-58.9937183934777,-1.27383087909548,
-4.9713812335004));
#44326=CARTESIAN_POINT('Ctrl Pts',(-58.8751862942275,1.24851163302018,-4.97789970493691));
#44327=CARTESIAN_POINT('Ctrl Pts',(-58.7961648947275,2.72815027040562,-4.18057472720697));
#44328=CARTESIAN_POINT('Ctrl Pts',(-58.7566541949775,3.3288632474416,-3.6296410951818));
#44329=CARTESIAN_POINT('Ctrl Pts',(-59.3088415259036,-4.92475008045824,
0.000102229393649578));
#44330=CARTESIAN_POINT('Ctrl Pts',(-59.2892276839357,-4.92444723141628,
-0.40457869844043));
#44331=CARTESIAN_POINT('Ctrl Pts',(-59.2696138419679,-4.8746433485405,-0.809333178910587));
#44332=CARTESIAN_POINT('Ctrl Pts',(-59.25,-4.77631074058413,-1.20178265305869));
#44333=CARTESIAN_POINT('',(-89.575,-2.36246668965802,-3.31495875354372));
#44334=CARTESIAN_POINT('Ctrl Pts',(-89.575,-2.36246668965807,-3.31495875354369));
#44335=CARTESIAN_POINT('Ctrl Pts',(-89.575,-2.45838582797249,-3.26042738788591));
#44336=CARTESIAN_POINT('Ctrl Pts',(-89.575,-2.55193566874186,-3.20204001451282));
#44337=CARTESIAN_POINT('Ctrl Pts',(-89.575,-2.64286961056085,-3.1399345520892));
#44338=CARTESIAN_POINT('Ctrl Pts',(-89.575,-2.74661604656181,-3.06907849709195));
#44339=CARTESIAN_POINT('Ctrl Pts',(-89.575,-2.84695857765234,-2.99338381919177));
#44340=CARTESIAN_POINT('Ctrl Pts',(-89.575,-2.94368691211655,-2.91320714995187));
#44341=CARTESIAN_POINT('Ctrl Pts',(-89.575,-2.99886142577539,-2.86747382107156));
#44342=CARTESIAN_POINT('Ctrl Pts',(-89.575,-3.05285970924591,-2.82028127789999));
#44343=CARTESIAN_POINT('Ctrl Pts',(-89.575,-3.10563962166236,-2.77168887175325));
#44344=CARTESIAN_POINT('Ctrl Pts',(-89.575,-3.14178581168165,-2.73841048485076));
#44345=CARTESIAN_POINT('Ctrl Pts',(-89.575,-3.17736051677501,-2.70447543873133));
#44346=CARTESIAN_POINT('Ctrl Pts',(-89.575,-3.2123494287601,-2.66990159034028));
#44347=CARTESIAN_POINT('Ctrl Pts',(-89.575,-3.2275095232409,-2.65492133578431));
#44348=CARTESIAN_POINT('Ctrl Pts',(-89.575,-3.24255591559887,-2.63982476295436));
#44349=CARTESIAN_POINT('Ctrl Pts',(-89.575,-3.25748199328786,-2.62461929378221));
#44350=CARTESIAN_POINT('Ctrl Pts',(-89.575,-3.3480487337272,-2.53235729378015));
#44351=CARTESIAN_POINT('Ctrl Pts',(-89.575,-3.43425145592165,-2.43602714319471));
#44352=CARTESIAN_POINT('Ctrl Pts',(-89.575,-3.51587104376023,-2.33600610480426));
#44353=CARTESIAN_POINT('Ctrl Pts',(-89.575,-3.59801431578674,-2.235343315608));
#44354=CARTESIAN_POINT('Ctrl Pts',(-89.575,-3.6755160971797,-2.1309416141852));
#44355=CARTESIAN_POINT('Ctrl Pts',(-89.575,-3.74812577356222,-2.02314026876673));
#44356=CARTESIAN_POINT('Ctrl Pts',(-89.575,-3.7758648375512,-1.98195693663194));
#44357=CARTESIAN_POINT('Ctrl Pts',(-89.575,-3.80288958155743,-1.94027700948081));
#44358=CARTESIAN_POINT('Ctrl Pts',(-89.575,-3.8291846840685,-1.89811791855068));
#44359=CARTESIAN_POINT('Ctrl Pts',(-89.575,-3.84379722111461,-1.87468955283935));
#44360=CARTESIAN_POINT('Ctrl Pts',(-89.575,-3.85818441792707,-1.85111319949648));
#44361=CARTESIAN_POINT('Ctrl Pts',(-89.575,-3.87234353149911,-1.82739175299238));
#44362=CARTESIAN_POINT('Ctrl Pts',(-89.575,-3.88684146846591,-1.80310265929821));
#44363=CARTESIAN_POINT('Ctrl Pts',(-89.575,-3.90110312921264,-1.77865622603159));
#44364=CARTESIAN_POINT('Ctrl Pts',(-89.575,-3.91510906401187,-1.75408492413592));
#44365=CARTESIAN_POINT('Ctrl Pts',(-89.575,-3.9483574032939,-1.69575572342643));
#44366=CARTESIAN_POINT('Ctrl Pts',(-89.575,-3.98018043165855,-1.63669813276525));
#44367=CARTESIAN_POINT('Ctrl Pts',(-89.575,-4.01055012113675,-1.57696270795028));
#44368=CARTESIAN_POINT('Ctrl Pts',(-89.575,-4.06930739859425,-1.46139053746715));
#44369=CARTESIAN_POINT('Ctrl Pts',(-89.575,-4.1226270049118,-1.34328346094576));
#44370=CARTESIAN_POINT('Ctrl Pts',(-89.575,-4.17052221117986,-1.22307026261548));
#44371=CARTESIAN_POINT('Ctrl Pts',(-89.575,-4.21917412213225,-1.10095779508101));
#44372=CARTESIAN_POINT('Ctrl Pts',(-89.575,-4.26222923077464,-0.976671519362465));
#44373=CARTESIAN_POINT('Ctrl Pts',(-89.575,-4.29966099444105,-0.850625465759895));
#44374=CARTESIAN_POINT('Ctrl Pts',(-89.575,-4.33321105482267,-0.73765048689121));
#44375=CARTESIAN_POINT('Ctrl Pts',(-89.575,-4.36224318317356,-0.623260954448138));
#44376=CARTESIAN_POINT('Ctrl Pts',(-89.575,-4.38670787296779,-0.507737782983998));
#44377=CARTESIAN_POINT('Ctrl Pts',(-89.575,-4.40505639031346,-0.421095404385893));
#44378=CARTESIAN_POINT('Ctrl Pts',(-89.575,-4.42083514843072,-0.333814983468863));
#44379=CARTESIAN_POINT('Ctrl Pts',(-89.575,-4.43401182496587,-0.246011295920075));
#44380=CARTESIAN_POINT('Ctrl Pts',(-89.575,-4.43670953231835,-0.228034938008987));
#44381=CARTESIAN_POINT('Ctrl Pts',(-89.575,-4.43929843122109,-0.210034488347497));
#44382=CARTESIAN_POINT('Ctrl Pts',(-89.575,-4.44177724376552,-0.192017850254865));
#44383=CARTESIAN_POINT('Ctrl Pts',(-89.575,-4.46034107829701,-0.0570911938942948));
#44384=CARTESIAN_POINT('Ctrl Pts',(-89.575,-4.47268850119797,0.0783965346303783));
#44385=CARTESIAN_POINT('Ctrl Pts',(-89.575,-4.47881882237079,0.213996674459185));
#44386=CARTESIAN_POINT('Ctrl Pts',(-89.575,-4.48386468385179,0.325609019570174));
#44387=CARTESIAN_POINT('Ctrl Pts',(-89.575,-4.48469780383174,0.437298380135437));
#44388=CARTESIAN_POINT('Ctrl Pts',(-89.575,-4.48129460116943,0.548827278861343));
#44389=CARTESIAN_POINT('Ctrl Pts',(-89.575,-4.47718033749732,0.683658889537804));
#44390=CARTESIAN_POINT('Ctrl Pts',(-89.575,-4.46687624340075,0.81825623328625));
#44391=CARTESIAN_POINT('Ctrl Pts',(-89.575,-4.45055932884642,0.95224187162625));
#44392=CARTESIAN_POINT('Ctrl Pts',(-89.575,-4.43410929567778,1.08732060771176));
#44393=CARTESIAN_POINT('Ctrl Pts',(-89.575,-4.41154788824619,1.22177838109377));
#44394=CARTESIAN_POINT('Ctrl Pts',(-89.575,-4.38300371631061,1.3552312292716));
#44395=CARTESIAN_POINT('Ctrl Pts',(-89.575,-4.37317942089486,1.40116285438693));
#44396=CARTESIAN_POINT('Ctrl Pts',(-89.575,-4.36264596032573,1.44697540796571));
#44397=CARTESIAN_POINT('Ctrl Pts',(-89.575,-4.35140716440663,1.49265305345994));
#44398=CARTESIAN_POINT('Ctrl Pts',(-89.575,-4.34684379106549,1.51119989346264));
#44399=CARTESIAN_POINT('Ctrl Pts',(-89.575,-4.34216363098046,1.52972638380862));
#44400=CARTESIAN_POINT('Ctrl Pts',(-89.575,-4.33736846843864,1.54822544889459));
#44401=CARTESIAN_POINT('Ctrl Pts',(-89.575,-4.30255455258104,1.6825326574052));
#44402=CARTESIAN_POINT('Ctrl Pts',(-89.575,-4.26178334036351,1.81501182220626));
#44403=CARTESIAN_POINT('Ctrl Pts',(-89.575,-4.21527927082535,1.94527034803996));
#44404=CARTESIAN_POINT('Ctrl Pts',(-89.575,-4.16622998832337,2.08265804970475));
#44405=CARTESIAN_POINT('Ctrl Pts',(-89.575,-4.11080349897274,2.21757625221622));
#44406=CARTESIAN_POINT('Ctrl Pts',(-89.575,-4.04920152128966,2.34956945526825));
#44407=CARTESIAN_POINT('Ctrl Pts',(-89.575,-3.98759954360659,2.48156265832028));
#44408=CARTESIAN_POINT('Ctrl Pts',(-89.575,-3.91982188875961,2.61063186325139));
#44409=CARTESIAN_POINT('Ctrl Pts',(-89.575,-3.84600984132568,2.73631219024261));
#44410=CARTESIAN_POINT('Ctrl Pts',(-89.575,-3.79539462233335,2.82249510339621));
#44411=CARTESIAN_POINT('Ctrl Pts',(-89.575,-3.74194059919316,2.90708427153108));
#44412=CARTESIAN_POINT('Ctrl Pts',(-89.575,-3.685757800253,2.98998307575975));
#44413=CARTESIAN_POINT('Ctrl Pts',(-89.575,-3.66117782571668,3.0262513026098));
#44414=CARTESIAN_POINT('Ctrl Pts',(-89.575,-3.63607538756102,3.06219590136944));
#44415=CARTESIAN_POINT('Ctrl Pts',(-89.575,-3.61045898680098,3.09780836070636));
#44416=CARTESIAN_POINT('Ctrl Pts',(-89.575,-3.59444414953696,3.12007252444251));
#44417=CARTESIAN_POINT('Ctrl Pts',(-89.575,-3.57822842220398,3.14220686647649));
#44418=CARTESIAN_POINT('Ctrl Pts',(-89.575,-3.561813801149,3.16420924915912));
#44419=CARTESIAN_POINT('Ctrl Pts',(-89.575,-3.55121738546721,3.17841282974219));
#44420=CARTESIAN_POINT('Ctrl Pts',(-89.575,-3.54054059736235,3.19255799856896));
#44421=CARTESIAN_POINT('Ctrl Pts',(-89.575,-3.52978895491108,3.20663801030847));
#44422=CARTESIAN_POINT('Ctrl Pts',(-89.575,-3.44442130591044,3.31843279008742));
#44423=CARTESIAN_POINT('Ctrl Pts',(-89.575,-3.35424955362964,3.42624081848301));
#44424=CARTESIAN_POINT('Ctrl Pts',(-89.575,-3.25965520939464,3.52983805565444));
#44425=CARTESIAN_POINT('Ctrl Pts',(-89.575,-3.16306466624511,3.63562147736009));
#44426=CARTESIAN_POINT('Ctrl Pts',(-89.575,-3.061862594744,3.73701515673525));
#44427=CARTESIAN_POINT('Ctrl Pts',(-89.575,-2.95640427239074,3.83376236101877));
#44428=CARTESIAN_POINT('Ctrl Pts',(-89.575,-2.85057033496809,3.9308541536386));
#44429=CARTESIAN_POINT('Ctrl Pts',(-89.575,-2.74044929333694,4.02326694680084));
#44430=CARTESIAN_POINT('Ctrl Pts',(-89.575,-2.62635571134329,4.11071350969491));
#44431=CARTESIAN_POINT('Ctrl Pts',(-89.575,-2.51324470319011,4.19740698285653));
#44432=CARTESIAN_POINT('Ctrl Pts',(-89.575,-2.39622873242727,4.27921996512691));
#44433=CARTESIAN_POINT('Ctrl Pts',(-89.575,-2.27557844519584,4.35583648142124));
#44434=CARTESIAN_POINT('Ctrl Pts',(-89.575,-2.2401621729428,4.37832686633806));
#44435=CARTESIAN_POINT('Ctrl Pts',(-89.575,-2.20443252938109,4.40036920957963));
#44436=CARTESIAN_POINT('Ctrl Pts',(-89.575,-2.16839587231077,4.42195480991672));
#44437=CARTESIAN_POINT('Ctrl Pts',(-89.575,-2.36246668965802,-3.31495875354372));
#44438=CARTESIAN_POINT('Ctrl Pts',(-89.541895102924,-1.90253119087213,-3.64205446939111));
#44439=CARTESIAN_POINT('Ctrl Pts',(-89.4692795060981,-0.743215608995184,
-4.14925109584965));
#44440=CARTESIAN_POINT('Ctrl Pts',(-89.357153209522,1.22652580399161,-4.06036256423134));
#44441=CARTESIAN_POINT('Ctrl Pts',(-89.2386211102719,3.0126043279509,-2.98581045744857));
#44442=CARTESIAN_POINT('Ctrl Pts',(-89.1200890110218,4.07114973607406,-1.19021168789138));
#44443=CARTESIAN_POINT('Ctrl Pts',(-89.0015569117718,4.14653236502477,0.892824265437017));
#44444=CARTESIAN_POINT('Ctrl Pts',(-88.8830248125217,3.22054554208703,2.76024400176603));
#44445=CARTESIAN_POINT('Ctrl Pts',(-88.7644927132716,1.51681193095975,3.96107892847728));
#44446=CARTESIAN_POINT('Ctrl Pts',(-88.6459606140215,-0.553225051728948,
4.20533047603355));
#44447=CARTESIAN_POINT('Ctrl Pts',(-88.5274285147713,-2.48966060894145,
3.43401418720049));
#44448=CARTESIAN_POINT('Ctrl Pts',(-88.4128374204063,-3.78046138336312,
1.88661678745238));
#44449=CARTESIAN_POINT('Ctrl Pts',(-88.3377570257912,-4.07029801574691,
0.60629401811437));
#44450=CARTESIAN_POINT('Ctrl Pts',(-88.3021873309261,-4.07075680315937,
-6.4153765865849E-5));
#44451=CARTESIAN_POINT('Origin',(-89.575,-4.52129938221115E-16,0.));
#44452=CARTESIAN_POINT('',(-89.575,-4.925,-6.03138548580071E-16));
#44453=CARTESIAN_POINT('Origin',(-89.575,0.,0.));
#44454=CARTESIAN_POINT('Origin',(-89.575,0.,0.));
#44455=CARTESIAN_POINT('',(-89.575,2.3623075609234,-3.3148866100674));
#44456=CARTESIAN_POINT('Ctrl Pts',(-89.575,2.168571653936,4.4220722318262));
#44457=CARTESIAN_POINT('Ctrl Pts',(-89.575,2.2821250990704,4.35420104629545));
#44458=CARTESIAN_POINT('Ctrl Pts',(-89.575,2.39275344608793,4.28182199486674));
#44459=CARTESIAN_POINT('Ctrl Pts',(-89.575,2.50014797438266,4.20502572098651));
#44460=CARTESIAN_POINT('Ctrl Pts',(-89.575,2.61779725504862,4.12089642200546));
#44461=CARTESIAN_POINT('Ctrl Pts',(-89.575,2.73156660582321,4.03146595669976));
#44462=CARTESIAN_POINT('Ctrl Pts',(-89.575,2.84115665380361,3.93705927886078));
#44463=CARTESIAN_POINT('Ctrl Pts',(-89.575,2.90277481127167,3.88397813099817));
#44464=CARTESIAN_POINT('Ctrl Pts',(-89.575,2.96307101504279,3.82932321285263));
#44465=CARTESIAN_POINT('Ctrl Pts',(-89.575,3.02198593446763,3.77314840125018));
#44466=CARTESIAN_POINT('Ctrl Pts',(-89.575,3.06760205276204,3.72965386919888));
#44467=CARTESIAN_POINT('Ctrl Pts',(-89.575,3.11239001077279,3.68524810911733));
#44468=CARTESIAN_POINT('Ctrl Pts',(-89.575,3.15632026306078,3.63995524989996));
#44469=CARTESIAN_POINT('Ctrl Pts',(-89.575,3.17039174259067,3.62544730814836));
#44470=CARTESIAN_POINT('Ctrl Pts',(-89.575,3.18437396240699,3.61084957134963));
#44471=CARTESIAN_POINT('Ctrl Pts',(-89.575,3.19825970699225,3.59616964172652));
#44472=CARTESIAN_POINT('Ctrl Pts',(-89.575,3.29600568509946,3.49283315366522));
#44473=CARTESIAN_POINT('Ctrl Pts',(-89.575,3.38906451000149,3.38533402227797));
#44474=CARTESIAN_POINT('Ctrl Pts',(-89.575,3.47715297643748,3.27398824380113));
#44475=CARTESIAN_POINT('Ctrl Pts',(-89.575,3.56454504164893,3.16352273194281));
#44476=CARTESIAN_POINT('Ctrl Pts',(-89.575,3.64704539656432,3.04927047926725));
#44477=CARTESIAN_POINT('Ctrl Pts',(-89.575,3.72433174854956,2.93151774737872));
#44478=CARTESIAN_POINT('Ctrl Pts',(-89.575,3.78010696130726,2.84653917735723));
#44479=CARTESIAN_POINT('Ctrl Pts',(-89.575,3.83316575613913,2.75973704453675));
#44480=CARTESIAN_POINT('Ctrl Pts',(-89.575,3.88337035803795,2.67121456473261));
#44481=CARTESIAN_POINT('Ctrl Pts',(-89.575,3.89316127494673,2.65395088348545));
#44482=CARTESIAN_POINT('Ctrl Pts',(-89.575,3.90284479422599,2.6366195765463));
#44483=CARTESIAN_POINT('Ctrl Pts',(-89.575,3.91241586666383,2.61922861666568));
#44484=CARTESIAN_POINT('Ctrl Pts',(-89.575,3.95192210597965,2.5474444537688));
#44485=CARTESIAN_POINT('Ctrl Pts',(-89.575,3.9894735885843,2.47471694815245));
#44486=CARTESIAN_POINT('Ctrl Pts',(-89.575,4.02501789616192,2.40110681671847));
#44487=CARTESIAN_POINT('Ctrl Pts',(-89.575,4.08529830421341,2.27626970321235));
#44488=CARTESIAN_POINT('Ctrl Pts',(-89.575,4.13980858439682,2.1488947134306));
#44489=CARTESIAN_POINT('Ctrl Pts',(-89.575,4.18848418123897,2.01939883110378));
#44490=CARTESIAN_POINT('Ctrl Pts',(-89.575,4.23727899932862,1.88958577422464));
#44491=CARTESIAN_POINT('Ctrl Pts',(-89.575,4.28021061669979,1.75764059664755));
#44492=CARTESIAN_POINT('Ctrl Pts',(-89.575,4.31716264794545,1.62397443606211));
#44493=CARTESIAN_POINT('Ctrl Pts',(-89.575,4.34940277263216,1.50735260125635));
#44494=CARTESIAN_POINT('Ctrl Pts',(-89.575,4.37709030380136,1.38942023503649));
#44495=CARTESIAN_POINT('Ctrl Pts',(-89.575,4.40011523782483,1.2704522302738));
#44496=CARTESIAN_POINT('Ctrl Pts',(-89.575,4.41738393834243,1.18122622670178));
#44497=CARTESIAN_POINT('Ctrl Pts',(-89.575,4.43202930683058,1.09141767980199));
#44498=CARTESIAN_POINT('Ctrl Pts',(-89.575,4.44399344956095,1.00114538980556));
#44499=CARTESIAN_POINT('Ctrl Pts',(-89.575,4.44662217637848,0.98131102348768));
#44500=CARTESIAN_POINT('Ctrl Pts',(-89.575,4.4491214272835,0.961454282731452));
#44501=CARTESIAN_POINT('Ctrl Pts',(-89.575,4.45149052360382,0.941576451469683));
#44502=CARTESIAN_POINT('Ctrl Pts',(-89.575,4.45339217003573,0.925620744405863));
#44503=CARTESIAN_POINT('Ctrl Pts',(-89.575,4.45520977888628,0.909652643593547));
#44504=CARTESIAN_POINT('Ctrl Pts',(-89.575,4.45694206893395,0.893682614227721));
#44505=CARTESIAN_POINT('Ctrl Pts',(-89.575,4.47150613737446,0.759416068626175));
#44506=CARTESIAN_POINT('Ctrl Pts',(-89.575,4.48006670618292,0.624824366933115));
#44507=CARTESIAN_POINT('Ctrl Pts',(-89.575,4.48254040861087,0.490290079290064));
#44508=CARTESIAN_POINT('Ctrl Pts',(-89.575,4.48441082620459,0.388565920505318));
#44509=CARTESIAN_POINT('Ctrl Pts',(-89.575,4.48280022621022,0.286874382300006));
#44510=CARTESIAN_POINT('Ctrl Pts',(-89.575,4.47765283391769,0.185382629909725));
#44511=CARTESIAN_POINT('Ctrl Pts',(-89.575,4.4708173232612,0.0506060448773163));
#44512=CARTESIAN_POINT('Ctrl Pts',(-89.575,4.45774630659774,-0.0838193207669723));
#44513=CARTESIAN_POINT('Ctrl Pts',(-89.575,4.43853463850383,-0.217474622726431));
#44514=CARTESIAN_POINT('Ctrl Pts',(-89.575,4.41948336180413,-0.350014084035258));
#44515=CARTESIAN_POINT('Ctrl Pts',(-89.575,4.3943931624653,-0.481797008446402));
#44516=CARTESIAN_POINT('Ctrl Pts',(-89.575,4.3633124492345,-0.612389322273228));
#44517=CARTESIAN_POINT('Ctrl Pts',(-89.575,4.35249258102604,-0.657851329986865));
#44518=CARTESIAN_POINT('Ctrl Pts',(-89.575,4.34094636247025,-0.703168770078569));
#44519=CARTESIAN_POINT('Ctrl Pts',(-89.575,4.32867469288774,-0.748322346754215));
#44520=CARTESIAN_POINT('Ctrl Pts',(-89.575,4.32188014371106,-0.773322872979495));
#44521=CARTESIAN_POINT('Ctrl Pts',(-89.575,4.31486140087328,-0.798278987057204));
#44522=CARTESIAN_POINT('Ctrl Pts',(-89.575,4.30762822556628,-0.823155012688862));
#44523=CARTESIAN_POINT('Ctrl Pts',(-89.575,4.27082651666219,-0.949721868202683));
#44524=CARTESIAN_POINT('Ctrl Pts',(-89.575,4.2284455418425,-1.07434621957789));
#44525=CARTESIAN_POINT('Ctrl Pts',(-89.575,4.18060902078101,-1.19664913006994));
#44526=CARTESIAN_POINT('Ctrl Pts',(-89.575,4.13330059472136,-1.31760186805133));
#44527=CARTESIAN_POINT('Ctrl Pts',(-89.575,4.08065599662557,-1.43628480391947));
#44528=CARTESIAN_POINT('Ctrl Pts',(-89.575,4.02275110722225,-1.5523066966709));
#44529=CARTESIAN_POINT('Ctrl Pts',(-89.575,3.9669831666924,-1.66404686372408));
#44530=CARTESIAN_POINT('Ctrl Pts',(-89.575,3.90633553434453,-1.77331917779089));
#44531=CARTESIAN_POINT('Ctrl Pts',(-89.575,3.84084200108773,-1.87974354780758));
#44532=CARTESIAN_POINT('Ctrl Pts',(-89.575,3.795406360387,-1.95357464528281));
#44533=CARTESIAN_POINT('Ctrl Pts',(-89.575,3.74763766691163,-2.02603439909253));
#44534=CARTESIAN_POINT('Ctrl Pts',(-89.575,3.69760992698782,-2.09702185867333));
#44535=CARTESIAN_POINT('Ctrl Pts',(-89.575,3.67228386786391,-2.13295857300696));
#44536=CARTESIAN_POINT('Ctrl Pts',(-89.575,3.64637878219349,-2.16851783129296));
#44537=CARTESIAN_POINT('Ctrl Pts',(-89.575,3.61990383706715,-2.20368564459669));
#44538=CARTESIAN_POINT('Ctrl Pts',(-89.575,3.6053546481366,-2.22301196076424));
#44539=CARTESIAN_POINT('Ctrl Pts',(-89.575,3.59063335678628,-2.24222004951615));
#44540=CARTESIAN_POINT('Ctrl Pts',(-89.575,3.57574145307651,-2.26130750712511));
#44541=CARTESIAN_POINT('Ctrl Pts',(-89.575,3.56574983489207,-2.27411410272612));
#44542=CARTESIAN_POINT('Ctrl Pts',(-89.575,3.55568331247211,-2.28686390445547));
#44543=CARTESIAN_POINT('Ctrl Pts',(-89.575,3.54554784644704,-2.29954960063716));
#44544=CARTESIAN_POINT('Ctrl Pts',(-89.575,3.46370593992855,-2.40198411706263));
#44545=CARTESIAN_POINT('Ctrl Pts',(-89.575,3.37727065960685,-2.50037261434585));
#44546=CARTESIAN_POINT('Ctrl Pts',(-89.575,3.2865623996527,-2.59443436453125));
#44547=CARTESIAN_POINT('Ctrl Pts',(-89.575,3.1982374123592,-2.68602473231175));
#44548=CARTESIAN_POINT('Ctrl Pts',(-89.575,3.1058601936877,-2.7735130490358));
#44549=CARTESIAN_POINT('Ctrl Pts',(-89.575,3.00969504058764,-2.85659863268242));
#44550=CARTESIAN_POINT('Ctrl Pts',(-89.575,2.90963765176844,-2.94304706311907));
#44551=CARTESIAN_POINT('Ctrl Pts',(-89.575,2.80547890527683,-3.02473006120895));
#44552=CARTESIAN_POINT('Ctrl Pts',(-89.575,2.69749236355891,-3.10125338927706));
#44553=CARTESIAN_POINT('Ctrl Pts',(-89.575,2.59715794701766,-3.17235413341945));
#44554=CARTESIAN_POINT('Ctrl Pts',(-89.575,2.4935182722296,-3.23900035352837));
#44555=CARTESIAN_POINT('Ctrl Pts',(-89.575,2.3867824989408,-3.30082548293148));
#44556=CARTESIAN_POINT('Ctrl Pts',(-89.575,2.37864216657838,-3.30554065092234));
#44557=CARTESIAN_POINT('Ctrl Pts',(-89.575,2.37048382328845,-3.31022775171822));
#44558=CARTESIAN_POINT('Ctrl Pts',(-89.575,2.36230756092335,-3.31488661006744));
#44559=CARTESIAN_POINT('Origin',(-89.575,0.,0.));
#44560=CARTESIAN_POINT('Origin',(-92.3478126690739,0.,0.));
#44561=CARTESIAN_POINT('Ctrl Pts',(-89.575,2.36230756092335,-3.31488661006744));
#44562=CARTESIAN_POINT('Ctrl Pts',(-89.53548930025,2.91092803106123,-2.9239199082961));
#44563=CARTESIAN_POINT('Ctrl Pts',(-89.4564679007499,3.80977362498712,-1.86473730182378));
#44564=CARTESIAN_POINT('Ctrl Pts',(-89.3379358014998,4.23793920928767,0.175536844418832));
#44565=CARTESIAN_POINT('Ctrl Pts',(-89.2194037022498,3.6426422996848,2.17296520226056));
#44566=CARTESIAN_POINT('Ctrl Pts',(-89.1008716029996,2.16767467238955,3.64585259348834));
#44567=CARTESIAN_POINT('Ctrl Pts',(-88.9823395037495,0.169217900166083,
4.23817423904527));
#44568=CARTESIAN_POINT('Ctrl Pts',(-88.8638074044995,-1.87010146406577,
3.80705007020246));
#44569=CARTESIAN_POINT('Ctrl Pts',(-88.7452753052494,-3.45780118263798,
2.45651375596413));
#44570=CARTESIAN_POINT('Ctrl Pts',(-88.6566103934409,-4.02080610100348,
1.00253375424179));
#44571=CARTESIAN_POINT('Ctrl Pts',(-88.6074561813824,-4.07063751740027,
0.164530271781952));
#44572=CARTESIAN_POINT('Ctrl Pts',(-88.5978126690739,-4.07047297420895,
0.000103779743357239));
#44573=CARTESIAN_POINT('Ctrl Pts',(-90.0683458050225,2.85821514250023,-4.01076441581681));
#44574=CARTESIAN_POINT('Ctrl Pts',(-90.0288351052725,3.52200480358096,-3.5377240015621));
#44575=CARTESIAN_POINT('Ctrl Pts',(-89.9498137057724,4.60954062229736,-2.25619241161589));
#44576=CARTESIAN_POINT('Ctrl Pts',(-89.8312816065224,5.12758889712364,0.212386428881554));
#44577=CARTESIAN_POINT('Ctrl Pts',(-89.7127495072722,4.40732424172653,2.62912507582186));
#44578=CARTESIAN_POINT('Ctrl Pts',(-89.5942174080223,2.62272393109418,4.41120845668343));
#44579=CARTESIAN_POINT('Ctrl Pts',(-89.4756853087721,0.204740979810431,
5.1278732655197));
#44580=CARTESIAN_POINT('Ctrl Pts',(-89.357153209522,-2.26268264599522,4.60624532508225));
#44581=CARTESIAN_POINT('Ctrl Pts',(-89.2386211102719,-4.18368034012819,
2.9721975796889));
#44582=CARTESIAN_POINT('Ctrl Pts',(-89.1200890110219,-5.09433739022707,
0.620393721358178));
#44583=CARTESIAN_POINT('Ctrl Pts',(-89.0015569117718,-4.77473548481351,
-1.88124040813632));
#44584=CARTESIAN_POINT('Ctrl Pts',(-88.8830248125217,-3.30205642110157,
-3.9285595414724));
#44585=CARTESIAN_POINT('Ctrl Pts',(-88.7644927132715,-1.03194581520415,
-5.02715134367899));
#44586=CARTESIAN_POINT('Ctrl Pts',(-88.6459606140217,1.4873750729016,-4.91170792667414));
#44587=CARTESIAN_POINT('Ctrl Pts',(-88.5274285147712,3.6475016047403,-3.61010981787875));
#44588=CARTESIAN_POINT('Ctrl Pts',(-88.4088964155215,4.92677306135157,-1.43668632685003));
#44589=CARTESIAN_POINT('Ctrl Pts',(-88.2903643162711,5.01625117196016,1.08369027345755));
#44590=CARTESIAN_POINT('Ctrl Pts',(-88.1718322170212,3.89432738802994,3.34236064934112));
#44591=CARTESIAN_POINT('Ctrl Pts',(-88.053300117771,1.83194120826945,4.7938660642741));
#44592=CARTESIAN_POINT('Ctrl Pts',(-87.934768018521,-0.672850460394772,
5.08767459077047));
#44593=CARTESIAN_POINT('Ctrl Pts',(-87.8162359192709,-3.01515179619869,
4.15283278082187));
#44594=CARTESIAN_POINT('Ctrl Pts',(-87.6977038200208,-4.62930765380767,
2.21510070074297));
#44595=CARTESIAN_POINT('Ctrl Pts',(-87.5791717207707,-5.12550671786203,
-0.257568149694912));
#44596=CARTESIAN_POINT('Ctrl Pts',(-87.4606396215207,-4.38391916567946,
-2.66803545976375));
#44597=CARTESIAN_POINT('Ctrl Pts',(-87.3421075222705,-2.58363502634467,
-4.43418431252969));
#44598=CARTESIAN_POINT('Ctrl Pts',(-87.2235754230205,-0.159414750969839,
-5.12949777300655));
#44599=CARTESIAN_POINT('Ctrl Pts',(-87.1050433237703,2.30330346343951,-4.58606079569274));
#44600=CARTESIAN_POINT('Ctrl Pts',(-86.9865112245203,4.20978434230453,-2.93511094468713));
#44601=CARTESIAN_POINT('Ctrl Pts',(-86.8679791252702,5.09962140372923,-0.57534511816609));
#44602=CARTESIAN_POINT('Ctrl Pts',(-86.7494470260202,4.7579230348759,1.92336394386835));
#44603=CARTESIAN_POINT('Ctrl Pts',(-86.6309149267699,3.26720784141955,3.95758934041028));
#44604=CARTESIAN_POINT('Ctrl Pts',(-86.51238282752,0.98747677869704,5.03607486817927));
#44605=CARTESIAN_POINT('Ctrl Pts',(-86.3938507282698,-1.5307254455619,4.89837116567092));
#44606=CARTESIAN_POINT('Ctrl Pts',(-86.2753186290198,-3.6792644201411,3.57773305223478));
#44607=CARTESIAN_POINT('Ctrl Pts',(-86.1567865297696,-4.93927773133401,
1.39308864007884));
#44608=CARTESIAN_POINT('Ctrl Pts',(-86.0382544305197,-5.0064778815977,-1.12798035773757));
#44609=CARTESIAN_POINT('Ctrl Pts',(-85.9197223312695,-3.86463633955352,
-3.37664721719212));
#44610=CARTESIAN_POINT('Ctrl Pts',(-85.8011902320194,-1.78950265668055,
-4.80986909469498));
#44611=CARTESIAN_POINT('Ctrl Pts',(-85.6826581327694,0.717787798196774,
-5.08152940984589));
#44612=CARTESIAN_POINT('Ctrl Pts',(-85.5641260335192,3.05173575665768,-4.12602342915134));
#44613=CARTESIAN_POINT('Ctrl Pts',(-85.4455939342692,4.6487033766519,-2.17410151149252));
#44614=CARTESIAN_POINT('Ctrl Pts',(-85.3270618350191,5.12303022393767,0.302856056551541));
#44615=CARTESIAN_POINT('Ctrl Pts',(-85.2085297357689,4.36016851707821,2.70667526109965));
#44616=CARTESIAN_POINT('Ctrl Pts',(-85.089997636519,2.54434589691626,4.45684467120116));
#44617=CARTESIAN_POINT('Ctrl Pts',(-84.9714655372688,0.114075287214313,
5.13070631543219));
#44618=CARTESIAN_POINT('Ctrl Pts',(-84.8529334380187,-2.3437439867514,4.5655256642511));
#44619=CARTESIAN_POINT('Ctrl Pts',(-84.7344013387686,-4.23555972228263,
2.89779128050072));
#44620=CARTESIAN_POINT('Ctrl Pts',(-84.6158692395186,-5.1045070030619,0.530253450776926));
#44621=CARTESIAN_POINT('Ctrl Pts',(-84.4973371402685,-4.74073900349125,
-1.96533818136869));
#44622=CARTESIAN_POINT('Ctrl Pts',(-84.3788050410184,-3.23210404492749,
-3.98630956012352));
#44623=CARTESIAN_POINT('Ctrl Pts',(-84.2602729417683,-0.942930624672344,
-5.0446052673548));
#44624=CARTESIAN_POINT('Ctrl Pts',(-84.1417408425183,1.57395626304328,-4.88465169161484));
#44625=CARTESIAN_POINT('Ctrl Pts',(-84.0232087432681,3.71073985481043,-3.54507689568087));
#44626=CARTESIAN_POINT('Ctrl Pts',(-83.9046766440181,4.95139660853339,-1.34938211466315));
#44627=CARTESIAN_POINT('Ctrl Pts',(-83.786144544768,4.996313547471,1.17218232443875));
#44628=CARTESIAN_POINT('Ctrl Pts',(-83.6676124455178,3.83464343467326,3.41067005077977));
#44629=CARTESIAN_POINT('Ctrl Pts',(-83.5490803462678,1.74692433148727,4.82549643523095));
#44630=CARTESIAN_POINT('Ctrl Pts',(-83.4305482470177,-0.762669071361281,
5.07498732549725));
#44631=CARTESIAN_POINT('Ctrl Pts',(-83.3120161477676,-3.08808135396581,
4.09889180360466));
#44632=CARTESIAN_POINT('Ctrl Pts',(-83.1934840485174,-4.66773600126614,
2.13293250921188));
#44633=CARTESIAN_POINT('Ctrl Pts',(-83.0749519492676,-5.12015358337118,
-0.348120308313184));
#44634=CARTESIAN_POINT('Ctrl Pts',(-82.9564198500172,-4.3360773069755,-2.7451036509212));
#44635=CARTESIAN_POINT('Ctrl Pts',(-82.8378877507673,-2.50485803520711,
-4.47915691730343));
#44636=CARTESIAN_POINT('Ctrl Pts',(-82.7193556515171,-0.0687269133315581,
-5.13151411161976));
#44637=CARTESIAN_POINT('Ctrl Pts',(-82.6008235522671,2.38400144627611,-4.5446339314099));
#44638=CARTESIAN_POINT('Ctrl Pts',(-82.482291453017,4.2610042736359,-2.86024527731897));
#44639=CARTESIAN_POINT('Ctrl Pts',(-82.3637593537669,5.10899390254251,-0.48512036666401));
#44640=CARTESIAN_POINT('Ctrl Pts',(-82.2452272545168,4.72318468523324,2.0071589113837));
#44641=CARTESIAN_POINT('Ctrl Pts',(-82.1266951552668,3.19674779714024,4.01471841949691));
#44642=CARTESIAN_POINT('Ctrl Pts',(-82.0081630560165,0.898310820773131,
5.05274164544861));
#44643=CARTESIAN_POINT('Ctrl Pts',(-81.8896309567667,-1.61706414286808,
4.87055069003692));
#44644=CARTESIAN_POINT('Ctrl Pts',(-81.7710988575164,-3.74192545317829,
3.51214384233125));
#44645=CARTESIAN_POINT('Ctrl Pts',(-81.6525667582665,-4.96312874493817,
1.30557019249725));
#44646=CARTESIAN_POINT('Ctrl Pts',(-81.5340346590162,-4.98575896420362,
-1.21629273500752));
#44647=CARTESIAN_POINT('Ctrl Pts',(-81.4155025597662,-3.80435101570306,
-3.444426485743));
#44648=CARTESIAN_POINT('Ctrl Pts',(-81.2969704605161,-1.70420955854852,
-4.84074686870948));
#44649=CARTESIAN_POINT('Ctrl Pts',(-81.178438361266,0.80749077441535,-5.06804884700245));
#44650=CARTESIAN_POINT('Ctrl Pts',(-81.059906262016,3.12418574921904,-4.07144002421078));
#44651=CARTESIAN_POINT('Ctrl Pts',(-80.9413741627658,4.68640404108277,-2.09159690908447));
#44652=CARTESIAN_POINT('Ctrl Pts',(-80.8228420635158,5.11687702083888,0.393357369297109));
#44653=CARTESIAN_POINT('Ctrl Pts',(-80.7043099642657,4.31164741707871,2.78331762778997));
#44654=CARTESIAN_POINT('Ctrl Pts',(-80.5857778650156,2.46517452550958,4.50111930803315));
#44655=CARTESIAN_POINT('Ctrl Pts',(-80.4672457657655,0.0233731713667585,
5.13192109849988));
#44656=CARTESIAN_POINT('Ctrl Pts',(-80.3487136665154,-2.42407269760731,
4.52338722895587));
#44657=CARTESIAN_POINT('Ctrl Pts',(-80.2301815672654,-4.28611600895748,
2.82247586776921));
#44658=CARTESIAN_POINT('Ctrl Pts',(-80.1116494680152,-5.11308175170773,
0.439949391053537));
#44659=CARTESIAN_POINT('Ctrl Pts',(-79.9931173687653,-4.70526145123102,
-2.04882286740397));
#44660=CARTESIAN_POINT('Ctrl Pts',(-79.874585269515,-3.16114185962938,-4.04281369958593));
#44661=CARTESIAN_POINT('Ctrl Pts',(-79.7560531702651,-0.853620852164372,
-5.0604833669543));
#44662=CARTESIAN_POINT('Ctrl Pts',(-79.6375210710149,1.6600457180465,-4.85606926231917));
#44663=CARTESIAN_POINT('Ctrl Pts',(-79.5189889717648,3.77281877930689,-3.47893646452364));
#44664=CARTESIAN_POINT('Ctrl Pts',(-79.4004568725147,4.97447322440563,-1.26165629557262));
#44665=CARTESIAN_POINT('Ctrl Pts',(-79.2819247732647,4.97481495573534,1.26030814400383));
#44666=CARTESIAN_POINT('Ctrl Pts',(-79.1633926740146,3.77376144961482,3.47791388563469));
#44667=CARTESIAN_POINT('Ctrl Pts',(-79.0448605747645,1.66136167237367,4.85561920359439));
#44668=CARTESIAN_POINT('Ctrl Pts',(-78.9263284755144,-0.852249402763529,
5.0607145170417));
#44669=CARTESIAN_POINT('Ctrl Pts',(-78.8077963762643,-3.16004612982402,
4.04367023367986));
#44670=CARTESIAN_POINT('Ctrl Pts',(-78.6892642770142,-4.70470602303032,
2.05009794270264));
#44671=CARTESIAN_POINT('Ctrl Pts',(-78.5707321777641,-5.11320082239203,
-0.438563712145908));
#44672=CARTESIAN_POINT('Ctrl Pts',(-78.452200078514,-4.28688069486741,-2.82131419484211));
#44673=CARTESIAN_POINT('Ctrl Pts',(-78.333667979264,-2.42529858960037,-4.522730152271));
#44674=CARTESIAN_POINT('Ctrl Pts',(-78.2151358800138,0.0219826423251478,
-5.13192719533143));
#44675=CARTESIAN_POINT('Ctrl Pts',(-78.0966037807639,2.46395411522516,-4.50178731500325));
#44676=CARTESIAN_POINT('Ctrl Pts',(-77.9780716815136,4.31089396507947,-2.78448580336584));
#44677=CARTESIAN_POINT('Ctrl Pts',(-77.8595395822637,5.11676822082183,-0.394744452022419));
#44678=CARTESIAN_POINT('Ctrl Pts',(-77.7410074830134,4.68697475041556,2.0903276005335));
#44679=CARTESIAN_POINT('Ctrl Pts',(-77.6224753837635,3.12528085889329,4.07059158394664));
#44680=CARTESIAN_POINT('Ctrl Pts',(-77.5039432845133,0.808880632638544,
5.06783309384885));
#44681=CARTESIAN_POINT('Ctrl Pts',(-77.3854111852633,-1.70293070733278,
4.84120196057697));
#44682=CARTESIAN_POINT('Ctrl Pts',(-77.2668790860132,-3.80335080595143,
3.44547060595366));
#44683=CARTESIAN_POINT('Ctrl Pts',(-77.1483469867631,-4.98556332054866,
1.21761716875768));
#44684=CARTESIAN_POINT('Ctrl Pts',(-77.0298148875131,-4.96321218223962,
-1.30417137017964));
#44685=CARTESIAN_POINT('Ctrl Pts',(-76.9112827882629,-3.74342128882646,
-3.51123787294802));
#44686=CARTESIAN_POINT('Ctrl Pts',(-76.7927506890129,-1.61728813305841,
-4.86989428648745));
#44687=CARTESIAN_POINT('Ctrl Pts',(-76.6742185897627,0.894735013697703,
-5.05342397500786));
#44688=CARTESIAN_POINT('Ctrl Pts',(-76.5556864905126,3.20009374497158,-4.01469986050394));
#44689=CARTESIAN_POINT('Ctrl Pts',(-76.4371543912626,4.71382864353052,-2.01022859740298));
#44690=CARTESIAN_POINT('Ctrl Pts',(-76.2791115922624,5.26141933163145,1.31995330641));
#44691=CARTESIAN_POINT('Ctrl Pts',(-76.0815580935124,2.70784920336926,5.1429724685161));
#44692=CARTESIAN_POINT('Ctrl Pts',(-75.8444938950121,-2.83874316080605,
5.07524718716688));
#44693=CARTESIAN_POINT('Ctrl Pts',(-75.607429696512,-5.79701303111296,0.394996271206378));
#44694=CARTESIAN_POINT('Ctrl Pts',(-75.3703654980119,-3.49950474856753,
-4.6408040950746));
#44695=CARTESIAN_POINT('Ctrl Pts',(-75.1333012995116,1.9774213757655,-5.46581264071833));
#44696=CARTESIAN_POINT('Ctrl Pts',(-74.8962371010115,5.65797660303749,-1.32902724184649));
#44697=CARTESIAN_POINT('Ctrl Pts',(-74.6591729025112,4.20372685543133,4.01387644762517));
#44698=CARTESIAN_POINT('Ctrl Pts',(-74.4221087040113,-1.06631748846821,
5.71331599545101));
#44699=CARTESIAN_POINT('Ctrl Pts',(-74.1850445055108,-5.3686615009571,2.22772906990762));
#44700=CARTESIAN_POINT('Ctrl Pts',(-73.9479803070108,-4.79746384525761,
-3.28145345655763));
#44701=CARTESIAN_POINT('Ctrl Pts',(-73.7109161085106,0.126862191859868,
-5.809069471218));
#44702=CARTESIAN_POINT('Ctrl Pts',(-73.4738519100104,4.93873592962991,-3.0700951387947));
#44703=CARTESIAN_POINT('Ctrl Pts',(-73.2367877115102,5.26253689341103,2.46745183652891));
#44704=CARTESIAN_POINT('Ctrl Pts',(-73.0392342127601,1.56152334963781,5.19484888547336));
#44705=CARTESIAN_POINT('Ctrl Pts',(-72.88119141376,-1.79039388404845,4.80163401711829));
#44706=CARTESIAN_POINT('Ctrl Pts',(-72.7626593145099,-3.86263253914205,
3.38208291058891));
#44707=CARTESIAN_POINT('Ctrl Pts',(-72.6441272152597,-5.00671250687666,
1.12715326793019));
#44708=CARTESIAN_POINT('Ctrl Pts',(-72.5255951160098,-4.93938671358823,
-1.39066536611891));
#44709=CARTESIAN_POINT('Ctrl Pts',(-72.4070630167596,-3.68036712056178,
-3.57727440993159));
#44710=CARTESIAN_POINT('Ctrl Pts',(-72.2885309175095,-1.53198670632987,
-4.89768872636437));
#44711=CARTESIAN_POINT('Ctrl Pts',(-72.1699988182594,0.986079090438097,
-5.03647507888746));
#44712=CARTESIAN_POINT('Ctrl Pts',(-72.0514667190094,3.26615150869236,-3.9584086918721));
#44713=CARTESIAN_POINT('Ctrl Pts',(-71.9329346197593,4.75739352015727,-1.92468602931411));
#44714=CARTESIAN_POINT('Ctrl Pts',(-71.8144025205092,5.09978115928234,0.573979330983468));
#44715=CARTESIAN_POINT('Ctrl Pts',(-71.6958704212591,4.21057761945873,2.93396189490852));
#44716=CARTESIAN_POINT('Ctrl Pts',(-71.577338322009,2.30454721399284,4.58544042890789));
#44717=CARTESIAN_POINT('Ctrl Pts',(-71.458806222759,-0.158025119865097,
5.12953879695887));
#44718=CARTESIAN_POINT('Ctrl Pts',(-71.3402741235088,-2.5824330026147,4.43488531467397));
#44719=CARTESIAN_POINT('Ctrl Pts',(-71.2217420242588,-4.38319607615567,
2.66922293363304));
#44720=CARTESIAN_POINT('Ctrl Pts',(-71.1032099250087,-5.12543666721089,
0.258957419581195));
#44721=CARTESIAN_POINT('Ctrl Pts',(-70.9846778257586,-4.6299078162659,-2.21384617619623));
#44722=CARTESIAN_POINT('Ctrl Pts',(-70.8661457265085,-3.01627710741838,
-4.15201544906907));
#44723=CARTESIAN_POINT('Ctrl Pts',(-70.7476136272584,-0.674229226436862,
-5.08749208647444));
#44724=CARTESIAN_POINT('Ctrl Pts',(-70.6290815280083,1.83064198501573,-4.79436234138692));
#44725=CARTESIAN_POINT('Ctrl Pts',(-70.5105494287582,3.8934214476962,-3.34341590771825));
#44726=CARTESIAN_POINT('Ctrl Pts',(-70.3920173295081,5.015957304304,-1.08504967117028));
#44727=CARTESIAN_POINT('Ctrl Pts',(-70.2734852302581,4.92716222717632,1.43535112214182));
#44728=CARTESIAN_POINT('Ctrl Pts',(-70.1549531310079,3.64847983031567,3.60912113987176));
#44729=CARTESIAN_POINT('Ctrl Pts',(-70.0364210317579,1.48870610788084,4.91130477429458));
#44730=CARTESIAN_POINT('Ctrl Pts',(-69.9178889325078,-1.03058338436781,
5.02743059189797));
#44731=CARTESIAN_POINT('Ctrl Pts',(-69.7993568332578,-3.30099166563435,
3.92945473177838));
#44732=CARTESIAN_POINT('Ctrl Pts',(-69.6808247340076,-4.77422543725906,
1.88253338368117));
#44733=CARTESIAN_POINT('Ctrl Pts',(-69.5622926347576,-5.09450542813289,
-0.619011235112431));
#44734=CARTESIAN_POINT('Ctrl Pts',(-69.4437605355075,-4.18448547359292,
-2.97106744917556));
#44735=CARTESIAN_POINT('Ctrl Pts',(-69.3252284362574,-2.26393126363252,
-4.60562435506688));
#44736=CARTESIAN_POINT('Ctrl Pts',(-69.2066963370073,0.203352074273813,
-5.12794387646976));
#44737=CARTESIAN_POINT('Ctrl Pts',(-69.0881642377571,2.62152680891723,-4.41188821894996));
#44738=CARTESIAN_POINT('Ctrl Pts',(-68.9696321385072,4.40661471397025,-2.63038157478856));
#44739=CARTESIAN_POINT('Ctrl Pts',(-68.851100039257,5.12752515991275,-0.213649715257704));
#44740=CARTESIAN_POINT('Ctrl Pts',(-68.732567940007,4.61016154506751,2.25467758110799));
#44741=CARTESIAN_POINT('Ctrl Pts',(-68.6140358407568,2.97946483496381,4.17851047187654));
#44742=CARTESIAN_POINT('Ctrl Pts',(-68.4955037415068,0.62924088606478,5.09325204301474));
#44743=CARTESIAN_POINT('Ctrl Pts',(-68.3769716422567,-1.8729418817384,4.7779963555866));
#44744=CARTESIAN_POINT('Ctrl Pts',(-68.2584395430066,-3.92281768327795,
3.30887622768375));
#44745=CARTESIAN_POINT('Ctrl Pts',(-68.1399074437565,-5.02535081346788,
1.04067750429541));
#44746=CARTESIAN_POINT('Ctrl Pts',(-68.0213753445064,-4.91428452393621,
-1.47884011447142));
#44747=CARTESIAN_POINT('Ctrl Pts',(-67.9028432452563,-3.6164408196592,-3.64122455559547));
#44748=CARTESIAN_POINT('Ctrl Pts',(-67.7843111460063,-1.44524306646015,
-4.92426978802113));
#44749=CARTESIAN_POINT('Ctrl Pts',(-67.6657790467562,1.07497432972823,-5.01812620973149));
#44750=CARTESIAN_POINT('Ctrl Pts',(-67.5472469475061,3.33559030281248,-3.9001279207421));
#44751=CARTESIAN_POINT('Ctrl Pts',(-67.428714848256,4.79067635247856,-1.8402664351043));
#44752=CARTESIAN_POINT('Ctrl Pts',(-67.3101827490059,5.0888357999539,0.664011044694645));
#44753=CARTESIAN_POINT('Ctrl Pts',(-67.1916506497558,4.15806449152427,3.00793287004445));
#44754=CARTESIAN_POINT('Ctrl Pts',(-67.0731185505057,2.22313947494855,4.625452555296));
#44755=CARTESIAN_POINT('Ctrl Pts',(-66.9545864512557,-0.248663637685085,
5.12594643569966));
#44756=CARTESIAN_POINT('Ctrl Pts',(-66.8360543520055,-2.66041561008952,
4.3885475100494));
#44757=CARTESIAN_POINT('Ctrl Pts',(-66.7175222527555,-4.42968928387048,
2.5913342730593));
#44758=CARTESIAN_POINT('Ctrl Pts',(-66.5989901535053,-5.12921309460808,
0.168325566892939));
#44759=CARTESIAN_POINT('Ctrl Pts',(-66.4804580542554,-4.59005521598732,
-2.29533299992755));
#44760=CARTESIAN_POINT('Ctrl Pts',(-66.3619259550051,-2.9424198293519,-4.20467906197435));
#44761=CARTESIAN_POINT('Ctrl Pts',(-66.2433938557551,-0.584203404690506,
-5.09861420861756));
#44762=CARTESIAN_POINT('Ctrl Pts',(-66.1248617565051,1.91509549147353,-4.76125715803154));
#44763=CARTESIAN_POINT('Ctrl Pts',(-66.006329657255,3.95190751588822,-3.2740781072288));
#44764=CARTESIAN_POINT('Ctrl Pts',(-65.8877975580048,5.0343518063684,-0.996224049139549));
#44765=CARTESIAN_POINT('Ctrl Pts',(-65.7692654587548,4.90102297818209,1.52221359660857));
#44766=CARTESIAN_POINT('Ctrl Pts',(-65.6507333595047,3.5841193383779,3.67304356557805));
#44767=CARTESIAN_POINT('Ctrl Pts',(-65.5322012602546,1.40166714072751,4.93685017931207));
#44768=CARTESIAN_POINT('Ctrl Pts',(-65.4136691610046,-1.11928131156664,
5.00842987491554));
#44769=CARTESIAN_POINT('Ctrl Pts',(-65.2951370617544,-3.36992840567857,
3.87049648068172));
#44770=CARTESIAN_POINT('Ctrl Pts',(-65.1766049625044,-4.80675308033382,
1.79785574812611));
#44771=CARTESIAN_POINT('Ctrl Pts',(-65.0580728632543,-5.08276869596689,
-0.708958990117128));
#44772=CARTESIAN_POINT('Ctrl Pts',(-64.9395407640041,-4.13131873377937,
-3.04456334903587));
#44773=CARTESIAN_POINT('Ctrl Pts',(-64.8210086647541,-2.1821740425865,-4.64491947338492));
#44774=CARTESIAN_POINT('Ctrl Pts',(-64.702476565504,0.293955778622967,-5.12354862049567));
#44775=CARTESIAN_POINT('Ctrl Pts',(-64.583944466254,2.69909661307265,-4.36486402304454));
#44776=CARTESIAN_POINT('Ctrl Pts',(-64.4654123670038,4.45241786218732,-2.55208456890519));
#44777=CARTESIAN_POINT('Ctrl Pts',(-64.3468802677538,5.13050039972244,-0.122988271053509));
#44778=CARTESIAN_POINT('Ctrl Pts',(-64.2283481685036,4.56959036955502,2.33580913621787));
#44779=CARTESIAN_POINT('Ctrl Pts',(-64.1098160692536,2.90514499893036,4.23051923545547));
#44780=CARTESIAN_POINT('Ctrl Pts',(-63.9912839700034,0.539120292697892,
5.10357813463948));
#44781=CARTESIAN_POINT('Ctrl Pts',(-63.8727518707535,-1.95709951804845,
4.74414607098299));
#44782=CARTESIAN_POINT('Ctrl Pts',(-63.7542197715032,-3.9806886752142,3.23902425699317));
#44783=CARTESIAN_POINT('Ctrl Pts',(-63.6356876722533,-5.04295957905816,
0.951692781497464));
#44784=CARTESIAN_POINT('Ctrl Pts',(-63.5171555730031,-4.88737862618744,
-1.56546818257512));
#44785=CARTESIAN_POINT('Ctrl Pts',(-63.398623473753,-3.55151791079645,-3.70457568361896));
#44786=CARTESIAN_POINT('Ctrl Pts',(-63.280091374503,-1.35798173439636,-4.94904496599238));
#44787=CARTESIAN_POINT('Ctrl Pts',(-63.1615592752529,1.16350086923399,-4.9983423445839));
#44788=CARTESIAN_POINT('Ctrl Pts',(-63.0430271760028,3.40400329214487,-3.84056272614266));
#44789=CARTESIAN_POINT('Ctrl Pts',(-62.9244950767527,4.82245436512648,-1.75530463528116));
#44790=CARTESIAN_POINT('Ctrl Pts',(-62.8059629775026,5.07630459005136,0.753851560584832));
#44791=CARTESIAN_POINT('Ctrl Pts',(-62.6874308782526,4.10425028940277,3.08095602505127));
#44792=CARTESIAN_POINT('Ctrl Pts',(-62.5688987790024,2.14103816625032,4.66402358881631));
#44793=CARTESIAN_POINT('Ctrl Pts',(-62.4503666797523,-0.339224959437705,
5.12075061814821));
#44794=CARTESIAN_POINT('Ctrl Pts',(-62.3318345805022,-2.73756679658748,
4.34083960778975));
#44795=CARTESIAN_POINT('Ctrl Pts',(-62.2133024812522,-4.47479867366276,
2.51263552801999));
#44796=CARTESIAN_POINT('Ctrl Pts',(-62.0947703820021,-5.13138697468224,
0.0776413689181762));
#44797=CARTESIAN_POINT('Ctrl Pts',(-61.976238282752,-4.54876860427843,-2.37610282849254));
#44798=CARTESIAN_POINT('Ctrl Pts',(-61.8577061835019,-2.86764325503598,
-4.25602897401029));
#44799=CARTESIAN_POINT('Ctrl Pts',(-61.7391740842518,-0.493995071621616,
-5.10814343336204));
#44800=CARTESIAN_POINT('Ctrl Pts',(-61.6206419850017,1.99895068105866,-4.7266644309417));
#44801=CARTESIAN_POINT('Ctrl Pts',(-61.5021098857517,4.00915891238501,-3.2037174149467));
#44802=CARTESIAN_POINT('Ctrl Pts',(-61.3835777865016,5.0511734609159,-0.907087179582999));
#44803=CARTESIAN_POINT('Ctrl Pts',(-61.2650456872514,4.87335253023417,1.60860049385013));
#44804=CARTESIAN_POINT('Ctrl Pts',(-61.1465135880015,3.51863909026266,3.73581844686004));
#44805=CARTESIAN_POINT('Ctrl Pts',(-61.0279814887513,1.31419024565512,4.96085319548998));
#44806=CARTESIAN_POINT('Ctrl Pts',(-60.9094493895012,-1.2076295207279,4.98786440678609));
#44807=CARTESIAN_POINT('Ctrl Pts',(-60.7909172902511,-3.43781235735713,
3.81032899489403));
#44808=CARTESIAN_POINT('Ctrl Pts',(-60.6723851910011,-4.83777886638368,
1.71261642068914));
#44809=CARTESIAN_POINT('Ctrl Pts',(-60.5538530917509,-5.06944421686892,
-0.798685250787317));
#44810=CARTESIAN_POINT('Ctrl Pts',(-60.4353209925009,-4.07686080989476,
-3.11710805327251));
#44811=CARTESIAN_POINT('Ctrl Pts',(-60.3167888932508,-2.09973599091779,
-4.68276341400958));
#44812=CARTESIAN_POINT('Ctrl Pts',(-60.1982567940008,0.384469521220488,
-5.11755263795289));
#44813=CARTESIAN_POINT('Ctrl Pts',(-60.0797246947506,2.77581937568727,-4.31647615939701));
#44814=CARTESIAN_POINT('Ctrl Pts',(-59.9611925955006,4.49683758333763,-2.47299019416017));
#44815=CARTESIAN_POINT('Ctrl Pts',(-59.8426604962504,5.13185741717796,-0.032288477837873));
#44816=CARTESIAN_POINT('Ctrl Pts',(-59.7241283970004,4.52762243183336,2.41621107972979));
#44817=CARTESIAN_POINT('Ctrl Pts',(-59.6055962977503,2.82985525829162,4.28120600452079));
#44818=CARTESIAN_POINT('Ctrl Pts',(-59.4870641985002,0.448957713397435,
5.11230993433101));
#44819=CARTESIAN_POINT('Ctrl Pts',(-59.3685320992501,-2.04091141443468,
4.70881615114383));
#44820=CARTESIAN_POINT('Ctrl Pts',(-59.28951069975,-3.3712993556795,3.68162322923883));
#44821=CARTESIAN_POINT('Ctrl Pts',(-59.25,-3.87448963569914,3.04038732119116));
#44822=CARTESIAN_POINT('Ctrl Pts',(-89.9038972033484,2.69291261530793,-3.77880514723369));
#44823=CARTESIAN_POINT('Ctrl Pts',(-89.8643865035983,3.31831254607438,-3.3331226371401));
#44824=CARTESIAN_POINT('Ctrl Pts',(-89.7853651040982,4.34295162319395,-2.12570737501852));
#44825=CARTESIAN_POINT('Ctrl Pts',(-89.6668330048482,4.83103900117832,0.200103234060647));
#44826=CARTESIAN_POINT('Ctrl Pts',(-89.548300905598,4.15243026104595,2.47707178463476));
#44827=CARTESIAN_POINT('Ctrl Pts',(-89.4297688063481,2.4710408448593,4.1560898356184));
#44828=CARTESIAN_POINT('Ctrl Pts',(-89.3112367070978,0.192899953262315,
4.83130692336156));
#44829=CARTESIAN_POINT('Ctrl Pts',(-89.1927046078479,-2.13182225201874,
4.33984690678899));
#44830=CARTESIAN_POINT('Ctrl Pts',(-89.0741725085977,-3.94172062096479,
2.80030297178065));
#44831=CARTESIAN_POINT('Ctrl Pts',(-88.9556404093478,-4.7997105678955,0.584513759605153));
#44832=CARTESIAN_POINT('Ctrl Pts',(-88.8371083100975,-4.49859257640246,
-1.77244041295852));
#44833=CARTESIAN_POINT('Ctrl Pts',(-88.7185762108475,-3.11108469779655,
-3.70135452433616));
#44834=CARTESIAN_POINT('Ctrl Pts',(-88.6000441115974,-0.972264075840879,
-4.73641017121377));
#44835=CARTESIAN_POINT('Ctrl Pts',(-88.4815120123473,1.40135395616427,-4.62764332949355));
#44836=CARTESIAN_POINT('Ctrl Pts',(-88.3629799130972,3.43655134272674,-3.40132207917299));
#44837=CARTESIAN_POINT('Ctrl Pts',(-88.2444478138472,4.64183718447002,-1.35359675214318));
#44838=CARTESIAN_POINT('Ctrl Pts',(-88.1259157145971,4.72614040198114,1.02101593581497));
#44839=CARTESIAN_POINT('Ctrl Pts',(-88.0073836153469,3.66910215939564,3.14905796407129));
#44840=CARTESIAN_POINT('Ctrl Pts',(-87.8888515160969,1.72599239185885,4.51661675449933));
#44841=CARTESIAN_POINT('Ctrl Pts',(-87.7703194168468,-0.63393670618787,
4.79343310597768));
#44842=CARTESIAN_POINT('Ctrl Pts',(-87.6517873175967,-2.84077296642872,
3.91265710493609));
#44843=CARTESIAN_POINT('Ctrl Pts',(-87.5332552183467,-4.36157544465854,
2.08699216952231));
#44844=CARTESIAN_POINT('Ctrl Pts',(-87.4147231190965,-4.82907724304558,
-0.242671907128827));
#44845=CARTESIAN_POINT('Ctrl Pts',(-87.2961910198465,-4.13037879836486,
-2.5137318184529));
#44846=CARTESIAN_POINT('Ctrl Pts',(-87.1776589205964,-2.43421261483795,
-4.17773690169677));
#44847=CARTESIAN_POINT('Ctrl Pts',(-87.0591268213463,-0.15019512967007,
-4.83283747879104));
#44848=CARTESIAN_POINT('Ctrl Pts',(-86.9405947220962,2.17009379782133,-4.32082973309242));
#44849=CARTESIAN_POINT('Ctrl Pts',(-86.8220626228462,3.96631491959732,-2.76536121187931));
#44850=CARTESIAN_POINT('Ctrl Pts',(-86.703530523596,4.80468898481305,-0.542070505409861));
#44851=CARTESIAN_POINT('Ctrl Pts',(-86.5849984243459,4.48275246070997,1.81212776856987));
#44852=CARTESIAN_POINT('Ctrl Pts',(-86.4664663250959,3.07825155712221,3.72870540867557));
#44853=CARTESIAN_POINT('Ctrl Pts',(-86.3479342258458,0.930366869566953,
4.74481761099761));
#44854=CARTESIAN_POINT('Ctrl Pts',(-86.2294021265957,-1.44219719559694,
4.61507788911824));
#44855=CARTESIAN_POINT('Ctrl Pts',(-86.1108700273456,-3.46647718176477,
3.37081779720027));
#44856=CARTESIAN_POINT('Ctrl Pts',(-85.9923379280955,-4.6536186571259,1.31252050180827));
#44857=CARTESIAN_POINT('Ctrl Pts',(-85.8738058288454,-4.71693234184641,
-1.062744539417));
#44858=CARTESIAN_POINT('Ctrl Pts',(-85.7552737295953,-3.6411282683421,-3.18136159640766));
#44859=CARTESIAN_POINT('Ctrl Pts',(-85.6367416303453,-1.68600823907419,
-4.53169426278861));
#44860=CARTESIAN_POINT('Ctrl Pts',(-85.5182095310951,0.676275129935608,
-4.78764332654887));
#44861=CARTESIAN_POINT('Ctrl Pts',(-85.3996774318452,2.87524112355692,-3.88739825011851));
#44862=CARTESIAN_POINT('Ctrl Pts',(-85.2811453325949,4.37984943178903,-2.04836413473647));
#44863=CARTESIAN_POINT('Ctrl Pts',(-85.162613233345,4.82674397511501,0.285340625057606));
#44864=CARTESIAN_POINT('Ctrl Pts',(-85.0440811340948,4.10800174903465,2.55013691858802));
#44865=CARTESIAN_POINT('Ctrl Pts',(-84.9255490348447,2.39719573996768,4.19908671712054));
#44866=CARTESIAN_POINT('Ctrl Pts',(-84.8070169355947,0.107477836593331,
4.83397612615729));
#44867=CARTESIAN_POINT('Ctrl Pts',(-84.6884848363446,-2.2081954766547,4.3014822341257));
#44868=CARTESIAN_POINT('Ctrl Pts',(-84.5699527370944,-3.99059960162677,
2.730199899845));
#44869=CARTESIAN_POINT('Ctrl Pts',(-84.4514206378445,-4.80929202951765,
0.499586677599988));
#44870=CARTESIAN_POINT('Ctrl Pts',(-84.3328885385942,-4.4665622536785,-1.85167446049024));
#44871=CARTESIAN_POINT('Ctrl Pts',(-84.2143564393443,-3.04517795989258,
-3.75576461805074));
#44872=CARTESIAN_POINT('Ctrl Pts',(-84.0958243400941,-0.88839700580379,
-4.75285466153723));
#44873=CARTESIAN_POINT('Ctrl Pts',(-83.9772922408441,1.48292779422635,-4.60215186958539));
#44874=CARTESIAN_POINT('Ctrl Pts',(-83.8587601415939,3.49613226050008,-3.34005028266161));
#44875=CARTESIAN_POINT('Ctrl Pts',(-83.740228042344,4.66503664900773,-1.27134170742255));
#44876=CARTESIAN_POINT('Ctrl Pts',(-83.6216959430937,4.70735585364263,1.10439012164805));
#44877=CARTESIAN_POINT('Ctrl Pts',(-83.5031638438438,3.61286997850212,3.21341674733537));
#44878=CARTESIAN_POINT('Ctrl Pts',(-83.3846317445935,1.64589239637687,4.54641780890914));
#44879=CARTESIAN_POINT('Ctrl Pts',(-83.2660996453436,-0.718560731498145,
4.78147959827983));
#44880=CARTESIAN_POINT('Ctrl Pts',(-83.1475675460934,-2.9094847030715,3.86183575986994));
#44881=CARTESIAN_POINT('Ctrl Pts',(-83.0290354468434,-4.39778132017769,
2.00957610791767));
#44882=CARTESIAN_POINT('Ctrl Pts',(-82.9105033475932,-4.82403370269499,
-0.327987055964406));
#44883=CARTESIAN_POINT('Ctrl Pts',(-82.7919712483432,-4.08530383429795,
-2.58634283402023));
#44884=CARTESIAN_POINT('Ctrl Pts',(-82.673439149093,-2.35999162633504,-4.22010855277988));
#44885=CARTESIAN_POINT('Ctrl Pts',(-82.5549070498431,-0.0647521486992605,
-4.83473720411525));
#44886=CARTESIAN_POINT('Ctrl Pts',(-82.4363749505929,2.24612467904481,-4.28179875750872));
#44887=CARTESIAN_POINT('Ctrl Pts',(-82.3178428513428,4.01457258823341,-2.6948253389454));
#44888=CARTESIAN_POINT('Ctrl Pts',(-82.1993107520927,4.81351943284894,-0.457063828368594));
#44889=CARTESIAN_POINT('Ctrl Pts',(-82.0807786528427,4.45002317501111,1.89107652290472));
#44890=CARTESIAN_POINT('Ctrl Pts',(-81.9622465535925,3.01186651168125,3.7825304743558));
#44891=CARTESIAN_POINT('Ctrl Pts',(-81.8437144543425,0.846357751646158,
4.76052047888104));
#44892=CARTESIAN_POINT('Ctrl Pts',(-81.7251823550923,-1.52354256519767,
4.58886638786185));
#44893=CARTESIAN_POINT('Ctrl Pts',(-81.6066502558424,-3.52551426537858,
3.30902188542618));
#44894=CARTESIAN_POINT('Ctrl Pts',(-81.4881181565922,-4.67609026693143,
1.23006361182116));
#44895=CARTESIAN_POINT('Ctrl Pts',(-81.3695860573422,-4.69741168603698,
-1.14594944282047));
#44896=CARTESIAN_POINT('Ctrl Pts',(-81.251053958092,-3.58432949672381,-3.24522090658449));
#44897=CARTESIAN_POINT('Ctrl Pts',(-81.132521858842,-1.60564799727745,-4.5607862460826));
#44898=CARTESIAN_POINT('Ctrl Pts',(-81.0139897595918,0.760790208138697,
-4.77494240099476));
#44899=CARTESIAN_POINT('Ctrl Pts',(-80.8954576603418,2.94350103025408,-3.83597163160921));
#44900=CARTESIAN_POINT('Ctrl Pts',(-80.7769255610917,4.41536970923133,-1.97063111830187));
#44901=CARTESIAN_POINT('Ctrl Pts',(-80.6583934618416,4.82094663746786,0.370607868649802));
#44902=CARTESIAN_POINT('Ctrl Pts',(-80.5398613625915,4.06228682703513,2.62234673689682));
#44903=CARTESIAN_POINT('Ctrl Pts',(-80.4213292633414,2.32260317985487,4.24080076666502));
#44904=CARTESIAN_POINT('Ctrl Pts',(-80.3027971640914,0.0220214031817654,
4.83512065324315));
#44905=CARTESIAN_POINT('Ctrl Pts',(-80.1842650648412,-2.28387844243946,
4.26178084065517));
#44906=CARTESIAN_POINT('Ctrl Pts',(-80.0657329655913,-4.03823200695045,
2.65924029220176));
#44907=CARTESIAN_POINT('Ctrl Pts',(-79.947200866341,-4.81737086461236,0.41450527906331));
#44908=CARTESIAN_POINT('Ctrl Pts',(-79.8286687670911,-4.43313651653883,
-1.93033087821979));
#44909=CARTESIAN_POINT('Ctrl Pts',(-79.7101366678409,-2.97831981434657,
-3.80900088697707));
#44910=CARTESIAN_POINT('Ctrl Pts',(-79.5916045685908,-0.804252390697374,
-4.76781446427664));
#44911=CARTESIAN_POINT('Ctrl Pts',(-79.4730724693408,1.56403833624816,-4.57522248163207));
#44912=CARTESIAN_POINT('Ctrl Pts',(-79.3545403700905,3.55462090134293,-3.27773502906268));
#44913=CARTESIAN_POINT('Ctrl Pts',(-79.2360082708407,4.68677864773865,-1.18868943908753));
#44914=CARTESIAN_POINT('Ctrl Pts',(-79.1174761715904,4.68710061531734,1.18741925675842));
#44915=CARTESIAN_POINT('Ctrl Pts',(-78.9989440723404,3.55550905308716,3.27677159018463));
#44916=CARTESIAN_POINT('Ctrl Pts',(-78.8804119730904,1.56527818343671,4.57479845168433));
#44917=CARTESIAN_POINT('Ctrl Pts',(-78.7618798738402,-0.802960257947215,
4.76803224598841));
#44918=CARTESIAN_POINT('Ctrl Pts',(-78.6433477745902,-2.97728745517533,
3.80980788412455));
#44919=CARTESIAN_POINT('Ctrl Pts',(-78.5248156753401,-4.43261321107233,
1.93153221058489));
#44920=CARTESIAN_POINT('Ctrl Pts',(-78.4062835760899,-4.81748304894133,
-0.413199739758205));
#44921=CARTESIAN_POINT('Ctrl Pts',(-78.2877514768399,-4.03895246787828,
-2.65814580367513));
#44922=CARTESIAN_POINT('Ctrl Pts',(-78.1692193775897,-2.28503343597506,
-4.26116176546116));
#44923=CARTESIAN_POINT('Ctrl Pts',(-78.0506872783397,0.020711294246199,
-4.83512639746945));
#44924=CARTESIAN_POINT('Ctrl Pts',(-77.9321551790896,2.32145335099778,-4.24143014000017));
#44925=CARTESIAN_POINT('Ctrl Pts',(-77.8136230798395,4.06157695031397,-2.62344735199687));
#44926=CARTESIAN_POINT('Ctrl Pts',(-77.6950909805894,4.82084412981051,-0.371914730583939));
#44927=CARTESIAN_POINT('Ctrl Pts',(-77.5765588813394,4.41590741205818,1.96943521916934));
#44928=CARTESIAN_POINT('Ctrl Pts',(-77.4580267820892,2.94453280515897,3.8351722601915));
#44929=CARTESIAN_POINT('Ctrl Pts',(-77.3394946828392,0.762099685052078,
4.77473912574775));
#44930=CARTESIAN_POINT('Ctrl Pts',(-77.220962583589,-1.60444310737234,4.5612150180854));
#44931=CARTESIAN_POINT('Ctrl Pts',(-77.102430484339,-3.58338713328238,3.24620464095956));
#44932=CARTESIAN_POINT('Ctrl Pts',(-76.9838983850889,-4.69722735727226,
1.14719727903154));
#44933=CARTESIAN_POINT('Ctrl Pts',(-76.8653662858388,-4.67616887870502,
-1.22874568924441));
#44934=CARTESIAN_POINT('Ctrl Pts',(-76.7468341865888,-3.52692359059955,
-3.30816831203879));
#44935=CARTESIAN_POINT('Ctrl Pts',(-76.6283020873386,-1.52375360109911,
-4.58824794687301));
#44936=CARTESIAN_POINT('Ctrl Pts',(-76.5097699880886,0.842988748438532,
-4.76116334647018));
#44937=CARTESIAN_POINT('Ctrl Pts',(-76.3912378888385,3.01501894936562,-3.78251298870692));
#44938=CARTESIAN_POINT('Ctrl Pts',(-76.2727057895883,4.44120823230232,-1.89396867615214));
#44939=CARTESIAN_POINT('Ctrl Pts',(-76.1146629905883,4.95712946233337,1.24361489014421));
#44940=CARTESIAN_POINT('Ctrl Pts',(-75.9171094918381,2.5512429668698,4.84553287634373));
#44941=CARTESIAN_POINT('Ctrl Pts',(-75.680045293338,-2.67456677969549,4.78172443106303));
#44942=CARTESIAN_POINT('Ctrl Pts',(-75.4429810948378,-5.46174753973659,
0.372151986012044));
#44943=CARTESIAN_POINT('Ctrl Pts',(-75.2059168963376,-3.2971137632781,-4.37240699867927));
#44944=CARTESIAN_POINT('Ctrl Pts',(-74.9688526978375,1.86305883325509,-5.14970185212314));
#44945=CARTESIAN_POINT('Ctrl Pts',(-74.7317884993372,5.33075216937959,-1.25216404197114));
#44946=CARTESIAN_POINT('Ctrl Pts',(-74.4947243008371,3.96060776250636,3.7817371972363));
#44947=CARTESIAN_POINT('Ctrl Pts',(-74.257660102337,-1.00464789158865,5.38289105344675));
#44948=CARTESIAN_POINT('Ctrl Pts',(-74.0205959038367,-5.05816936880361,
2.09889018731971));
#44949=CARTESIAN_POINT('Ctrl Pts',(-73.7835317053366,-4.52000646077214,
-3.09167328879938));
#44950=CARTESIAN_POINT('Ctrl Pts',(-73.5464675068364,0.119525221102254,
-5.47310670552218));
#44951=CARTESIAN_POINT('Ctrl Pts',(-73.3094033083362,4.65310819007873,-2.8925387058945));
#44952=CARTESIAN_POINT('Ctrl Pts',(-73.0723391098361,4.95818239084454,2.3247487844603));
#44953=CARTESIAN_POINT('Ctrl Pts',(-72.8747856110859,1.47121392816465,4.89440906329828));
#44954=CARTESIAN_POINT('Ctrl Pts',(-72.7167428120858,-1.6868479230387,4.52393545416548));
#44955=CARTESIAN_POINT('Ctrl Pts',(-72.5982107128358,-3.63924035608306,
3.18648292093757));
#44956=CARTESIAN_POINT('Ctrl Pts',(-72.4796786135856,-4.71715339776492,
1.06196528366983));
#44957=CARTESIAN_POINT('Ctrl Pts',(-72.3611465143356,-4.65372133648087,
-1.31023737590922));
#44958=CARTESIAN_POINT('Ctrl Pts',(-72.2426144150854,-3.4675161084115,-3.37038568009834));
#44959=CARTESIAN_POINT('Ctrl Pts',(-72.1240823158354,-1.44338551238339,
-4.61443491812896));
#44960=CARTESIAN_POINT('Ctrl Pts',(-72.0055502165852,0.929050015461517,
-4.7451946758479));
#44961=CARTESIAN_POINT('Ctrl Pts',(-71.8870181173353,3.07725631653146,-3.72947737361796));
#44962=CARTESIAN_POINT('Ctrl Pts',(-71.768486018085,4.48225357004057,-1.81337339228878));
#44963=CARTESIAN_POINT('Ctrl Pts',(-71.6499539188351,4.80483950103485,0.540783707408174));
#44964=CARTESIAN_POINT('Ctrl Pts',(-71.5314218195849,3.96706231821827,2.76427861645173));
#44965=CARTESIAN_POINT('Ctrl Pts',(-71.4128897203349,2.17126561708203,4.32024524471151));
#44966=CARTESIAN_POINT('Ctrl Pts',(-71.2943576210847,-0.148885866739932,
4.83287613015675));
#44967=CARTESIAN_POINT('Ctrl Pts',(-71.1758255218347,-2.43308010916401,
4.17839736195729));
#44968=CARTESIAN_POINT('Ctrl Pts',(-71.0572934225846,-4.12969752813031,
2.5148506157454));
#44969=CARTESIAN_POINT('Ctrl Pts',(-70.9387613233345,-4.82901124371636,
0.243980829731282));
#44970=CARTESIAN_POINT('Ctrl Pts',(-70.8202292240844,-4.36214089721349,
-2.08581019937327));
#44971=CARTESIAN_POINT('Ctrl Pts',(-70.7016971248343,-2.84183319619745,
-3.91188704289449));
#44972=CARTESIAN_POINT('Ctrl Pts',(-70.5831650255843,-0.63523573242734,
-4.79326115666786));
#44973=CARTESIAN_POINT('Ctrl Pts',(-70.4646329263341,1.72476830811586,-4.51708432983258));
#44974=CARTESIAN_POINT('Ctrl Pts',(-70.3461008270841,3.66824861337767,-3.15005219244613));
#44975=CARTESIAN_POINT('Ctrl Pts',(-70.227568727834,4.72586352991972,-1.02229671387652));
#44976=CARTESIAN_POINT('Ctrl Pts',(-70.1090366285839,4.64220384320865,1.35233876790359));
#44977=CARTESIAN_POINT('Ctrl Pts',(-69.9905045293338,3.4374729934287,3.40039058054721));
#44978=CARTESIAN_POINT('Ctrl Pts',(-69.8719724300837,1.40260801182774,4.62726349310103));
#44979=CARTESIAN_POINT('Ctrl Pts',(-69.7534403308337,-0.970980440073939,
4.73667326934116));
#44980=CARTESIAN_POINT('Ctrl Pts',(-69.6349082315835,-3.11008152158803,
3.7021979420454));
#44981=CARTESIAN_POINT('Ctrl Pts',(-69.5163761323335,-4.49811202702977,
1.77365861032375));
#44982=CARTESIAN_POINT('Ctrl Pts',(-69.3978440330833,-4.79986888746694,
-0.583211228316955));
#44983=CARTESIAN_POINT('Ctrl Pts',(-69.2793119338334,-3.94247919019627,
-2.79923820143815));
#44984=CARTESIAN_POINT('Ctrl Pts',(-69.1607798345832,-2.13299865687961,
-4.33926185006489));
#44985=CARTESIAN_POINT('Ctrl Pts',(-69.0422477353331,0.191591373937665,
-4.83137345058526));
#44986=CARTESIAN_POINT('Ctrl Pts',(-68.923715636083,2.4699129572611,-4.15673028439206));
#44987=CARTESIAN_POINT('Ctrl Pts',(-68.805183536833,4.15176176824522,-2.47825561501481));
#44988=CARTESIAN_POINT('Ctrl Pts',(-68.6866514375828,4.83097895015671,-0.201293459305886));
#44989=CARTESIAN_POINT('Ctrl Pts',(-68.5681193383328,4.34353663540522,2.12428015348995));
#44990=CARTESIAN_POINT('Ctrl Pts',(-68.4495872390826,2.80714993131055,3.93684974780085));
#44991=CARTESIAN_POINT('Ctrl Pts',(-68.3310551398326,0.592849255801311,
4.79868799084851));
#44992=CARTESIAN_POINT('Ctrl Pts',(-68.2125230405825,-1.76462182502469,
4.5016648573904));
#44993=CARTESIAN_POINT('Ctrl Pts',(-68.0939909413324,-3.69594474179837,
3.11751008646168));
#44994=CARTESIAN_POINT('Ctrl Pts',(-67.9754588420824,-4.73471377318983,
0.980490774859142));
#44995=CARTESIAN_POINT('Ctrl Pts',(-67.8569267428322,-4.63007091136744,
-1.39331261005075));
#44996=CARTESIAN_POINT('Ctrl Pts',(-67.7383946435822,-3.40728693266096,
-3.43063732156799));
#44997=CARTESIAN_POINT('Ctrl Pts',(-67.6198625443321,-1.36165861973998,
-4.63947868589835));
#44998=CARTESIAN_POINT('Ctrl Pts',(-67.501330445082,1.01280407153856,-4.72790699848171));
#44999=CARTESIAN_POINT('Ctrl Pts',(-67.3827983458318,3.1426791749781,-3.67456722305856));
#45000=CARTESIAN_POINT('Ctrl Pts',(-67.2642662465818,4.51361151706789,-1.73383613603175));
#45001=CARTESIAN_POINT('Ctrl Pts',(-67.1457341473317,4.79452715758092,0.625608510840759));
#45002=CARTESIAN_POINT('Ctrl Pts',(-67.0272020480816,3.91758624394338,2.83397154094444));
#45003=CARTESIAN_POINT('Ctrl Pts',(-66.9086699488316,2.09456602781867,4.35794330260563));
#45004=CARTESIAN_POINT('Ctrl Pts',(-66.7901378495815,-0.234282380263663,
4.82949153016292));
#45005=CARTESIAN_POINT('Ctrl Pts',(-66.6716057503314,-2.50655265653141,
4.13473946623638));
#45006=CARTESIAN_POINT('Ctrl Pts',(-66.5530736510812,-4.17350183933125,
2.44146658193717));
#45007=CARTESIAN_POINT('Ctrl Pts',(-66.4345415518312,-4.83256926453413,
0.158590595866855));
#45008=CARTESIAN_POINT('Ctrl Pts',(-66.3160094525811,-4.32459313936726,
-2.16258429952568));
#45009=CARTESIAN_POINT('Ctrl Pts',(-66.197477353331,-2.77224739319749,-3.96150489896542));
#45010=CARTESIAN_POINT('Ctrl Pts',(-66.0789452540809,-0.550416480202624,
-4.80374004000411));
#45011=CARTESIAN_POINT('Ctrl Pts',(-65.9604131548309,1.80433751533385,-4.48589375758903));
#45012=CARTESIAN_POINT('Ctrl Pts',(-65.8418810555807,3.723352187812,-3.08472448674641));
#45013=CARTESIAN_POINT('Ctrl Pts',(-65.7233489563307,4.74319420105255,-0.938608248801809));
#45014=CARTESIAN_POINT('Ctrl Pts',(-65.6048168570806,4.61757633622901,1.43417762244263));
#45015=CARTESIAN_POINT('Ctrl Pts',(-65.4862847578305,3.37683473772516,3.46061610522028));
#45016=CARTESIAN_POINT('Ctrl Pts',(-65.3677526585804,1.32060287191181,4.65133150058299));
#45017=CARTESIAN_POINT('Ctrl Pts',(-65.2492205593303,-1.05454859544256,
4.71877144323261));
#45018=CARTESIAN_POINT('Ctrl Pts',(-65.1306884600802,-3.17503136184424,
3.64664949301723));
#45019=CARTESIAN_POINT('Ctrl Pts',(-65.0121563608302,-4.52875846056089,
1.69387823633091));
#45020=CARTESIAN_POINT('Ctrl Pts',(-64.8936242615801,-4.78881093957408,
-0.667956928725949));
#45021=CARTESIAN_POINT('Ctrl Pts',(-64.77509216233,-3.89238730514893,-2.86848352624393));
#45022=CARTESIAN_POINT('Ctrl Pts',(-64.6565600630799,-2.05596979761929,
-4.37628436746227));
#45023=CARTESIAN_POINT('Ctrl Pts',(-64.5380279638298,0.276955087399081,
-4.82723239063349));
#45024=CARTESIAN_POINT('Ctrl Pts',(-64.4194958645797,2.5429965754503,-4.11242569426676));
#45025=CARTESIAN_POINT('Ctrl Pts',(-64.3009637653297,4.19491592897319,-2.40448685221282));
#45026=CARTESIAN_POINT('Ctrl Pts',(-64.1824316660795,4.83378211941362,-0.115875345326565));
#45027=CARTESIAN_POINT('Ctrl Pts',(-64.0638995668295,4.30531186053404,2.2007195316901));
#45028=CARTESIAN_POINT('Ctrl Pts',(-63.9453674675794,2.73712832200404,3.98585062721882));
#45029=CARTESIAN_POINT('Ctrl Pts',(-63.8268353683293,0.507940712994964,
4.80841688143817));
#45030=CARTESIAN_POINT('Ctrl Pts',(-63.7083032690792,-1.84391227350212,
4.46977227621784));
#45031=CARTESIAN_POINT('Ctrl Pts',(-63.5897711698291,-3.75046881240742,
3.05169794717246));
#45032=CARTESIAN_POINT('Ctrl Pts',(-63.4712390705791,-4.75130415027271,
0.896652410479528));
#45033=CARTESIAN_POINT('Ctrl Pts',(-63.3527069713289,-4.60472109413483,
-1.47493061492638));
#45034=CARTESIAN_POINT('Ctrl Pts',(-63.2341748720789,-3.34611878695376,
-3.4903245890909));
#45035=CARTESIAN_POINT('Ctrl Pts',(-63.1156427728288,-1.2794439752057,-4.66282101178322));
#45036=CARTESIAN_POINT('Ctrl Pts',(-62.9971106735787,1.09621075128068,-4.70926731693943));
#45037=CARTESIAN_POINT('Ctrl Pts',(-62.8785785743286,3.20713555521509,-3.61844693260701));
#45038=CARTESIAN_POINT('Ctrl Pts',(-62.7600464750785,4.54355167443271,-1.65378803217808));
#45039=CARTESIAN_POINT('Ctrl Pts',(-62.6415143758284,4.78272067991945,0.710253174221426));
#45040=CARTESIAN_POINT('Ctrl Pts',(-62.5229822765784,3.86688434203933,2.90277146170738));
#45041=CARTESIAN_POINT('Ctrl Pts',(-62.4044501773282,2.01721298093314,4.39428361205534));
#45042=CARTESIAN_POINT('Ctrl Pts',(-62.2859180780782,-0.319606162291232,
4.82459620845565));
#45043=CARTESIAN_POINT('Ctrl Pts',(-62.1673859788281,-2.57924186747184,
4.08979071135275));
#45044=CARTESIAN_POINT('Ctrl Pts',(-62.048853879578,-4.2160023645836,2.36731931423363));
#45045=CARTESIAN_POINT('Ctrl Pts',(-61.9303217803279,-4.83461742003818,
0.0731510440626118));
#45046=CARTESIAN_POINT('Ctrl Pts',(-61.8117896810779,-4.28569430496499,
-2.2386828713388));
#45047=CARTESIAN_POINT('Ctrl Pts',(-61.6932575818277,-2.70179546069225,
-4.00988503097871));
#45048=CARTESIAN_POINT('Ctrl Pts',(-61.5747254825777,-0.465425272047941,
-4.81271814985559));
#45049=CARTESIAN_POINT('Ctrl Pts',(-61.4561933833275,1.88334300884449,-4.45330167248215));
#45050=CARTESIAN_POINT('Ctrl Pts',(-61.3376612840775,3.77729249677535,-3.01843304736144));
#45051=CARTESIAN_POINT('Ctrl Pts',(-61.2191291848274,4.75904298901387,-0.854626536946514));
#45052=CARTESIAN_POINT('Ctrl Pts',(-61.1005970855773,4.59150618593059,1.51556840437503));
#45053=CARTESIAN_POINT('Ctrl Pts',(-60.9820649863272,3.31514148602376,3.51976045275908));
#45054=CARTESIAN_POINT('Ctrl Pts',(-60.8635328870771,1.23818513127863,4.67394632201816));
#45055=CARTESIAN_POINT('Ctrl Pts',(-60.745000787827,-1.13778725842931,4.69939536207552));
#45056=CARTESIAN_POINT('Ctrl Pts',(-60.626468688577,-3.23898930088597,3.58996174439405));
#45057=CARTESIAN_POINT('Ctrl Pts',(-60.5079365893268,-4.55798989573565,
1.6135686554452));
#45058=CARTESIAN_POINT('Ctrl Pts',(-60.3894044900768,-4.7762570707901,-0.752493944743505));
#45059=CARTESIAN_POINT('Ctrl Pts',(-60.2708723908267,-3.84107891060167,
-2.93683266704434));
#45060=CARTESIAN_POINT('Ctrl Pts',(-60.1523402915766,-1.97829948301663,
-4.41193963483726));
#45061=CARTESIAN_POINT('Ctrl Pts',(-60.0338081923265,0.362234041972942,
-4.82158318082052));
#45062=CARTESIAN_POINT('Ctrl Pts',(-59.9152760930764,2.6152821400511,-4.06683630300412));
#45063=CARTESIAN_POINT('Ctrl Pts',(-59.7967439938263,4.2367666720035,-2.32996683572293));
#45064=CARTESIAN_POINT('Ctrl Pts',(-59.6782118945763,4.83506065487822,-0.030421100219405));
#45065=CARTESIAN_POINT('Ctrl Pts',(-59.5596797953262,4.26577110404982,2.27647149478029));
#45066=CARTESIAN_POINT('Ctrl Pts',(-59.4411476960761,2.66619290172915,4.03360596859099));
#45067=CARTESIAN_POINT('Ctrl Pts',(-59.322615596826,0.422992612477064,4.81664368466023));
#45068=CARTESIAN_POINT('Ctrl Pts',(-59.204083497576,-1.9228769776405,4.43648563329933));
#45069=CARTESIAN_POINT('Ctrl Pts',(-59.1250620980759,-3.17632302407693,
3.46869957107404));
#45070=CARTESIAN_POINT('Ctrl Pts',(-59.0855513983258,-3.65041170719121,
2.86454901554256));
#45071=CARTESIAN_POINT('Ctrl Pts',(-89.7394486016742,2.52761008811564,-3.54684587865056));
#45072=CARTESIAN_POINT('Ctrl Pts',(-89.6999379019242,3.11462028856781,-3.1285212727181));
#45073=CARTESIAN_POINT('Ctrl Pts',(-89.620916502424,4.07636262409054,-1.99522233842116));
#45074=CARTESIAN_POINT('Ctrl Pts',(-89.5023844031741,4.53448910523299,0.187820039239741));
#45075=CARTESIAN_POINT('Ctrl Pts',(-89.3838523039238,3.89753628036537,2.32501849344766));
#45076=CARTESIAN_POINT('Ctrl Pts',(-89.2653202046739,2.31935775862443,3.90097121455338));
#45077=CARTESIAN_POINT('Ctrl Pts',(-89.1467881054237,0.181058926714198,
4.53474058120341));
#45078=CARTESIAN_POINT('Ctrl Pts',(-89.0282560061737,-2.00096185804225,
4.07344848849573));
#45079=CARTESIAN_POINT('Ctrl Pts',(-88.9097239069235,-3.69976090180139,
2.62840836387239));
#45080=CARTESIAN_POINT('Ctrl Pts',(-88.7911918076736,-4.50508374556393,
0.548633797852129));
#45081=CARTESIAN_POINT('Ctrl Pts',(-88.6726597084233,-4.22244966799141,
-1.66364041778071));
#45082=CARTESIAN_POINT('Ctrl Pts',(-88.5541276091733,-2.92011297449154,
-3.47414950719992));
#45083=CARTESIAN_POINT('Ctrl Pts',(-88.4355955099232,-0.912582336477606,
-4.44566899874856));
#45084=CARTESIAN_POINT('Ctrl Pts',(-88.3170634106731,1.31533283942694,-4.34357873231296));
#45085=CARTESIAN_POINT('Ctrl Pts',(-88.198531311423,3.22560108071319,-3.19253434046722));
#45086=CARTESIAN_POINT('Ctrl Pts',(-88.079999212173,4.35690130758848,-1.27050717743633));
#45087=CARTESIAN_POINT('Ctrl Pts',(-87.9614671129229,4.43602963200212,0.958341598172394));
#45088=CARTESIAN_POINT('Ctrl Pts',(-87.8429350136728,3.44387693076133,2.95575527880146));
#45089=CARTESIAN_POINT('Ctrl Pts',(-87.7244029144227,1.62004357544825,4.23936744472458));
#45090=CARTESIAN_POINT('Ctrl Pts',(-87.6058708151726,-0.595022951980973,
4.4991916211849));
#45091=CARTESIAN_POINT('Ctrl Pts',(-87.4873387159225,-2.66639413665873,
3.67248142905029));
#45092=CARTESIAN_POINT('Ctrl Pts',(-87.3688066166724,-4.0938432355094,1.95888363830165));
#45093=CARTESIAN_POINT('Ctrl Pts',(-87.2502745174224,-4.53264776822913,
-0.227775664562744));
#45094=CARTESIAN_POINT('Ctrl Pts',(-87.1317424181724,-3.87683843105025,
-2.35942817714205));
#45095=CARTESIAN_POINT('Ctrl Pts',(-87.013210318922,-2.28479020333122,-3.92128949086385));
#45096=CARTESIAN_POINT('Ctrl Pts',(-86.8946782196722,-0.140975508370298,
-4.53617718457553));
#45097=CARTESIAN_POINT('Ctrl Pts',(-86.776146120422,2.03688413220314,-4.05559867049211));
#45098=CARTESIAN_POINT('Ctrl Pts',(-86.657614021172,3.72284549689011,-2.5956114790715));
#45099=CARTESIAN_POINT('Ctrl Pts',(-86.5390819219218,4.50975656589686,-0.508795892653628));
#45100=CARTESIAN_POINT('Ctrl Pts',(-86.4205498226717,4.20758188654404,1.70089159327138));
#45101=CARTESIAN_POINT('Ctrl Pts',(-86.3020177234218,2.88929527282486,3.49982147694086));
#45102=CARTESIAN_POINT('Ctrl Pts',(-86.1834856241715,0.873256960436869,
4.45356035381594));
#45103=CARTESIAN_POINT('Ctrl Pts',(-86.0649535249215,-1.35366894563198,
4.33178461256555));
#45104=CARTESIAN_POINT('Ctrl Pts',(-85.9464214256714,-3.25368994338844,
3.16390254216576));
#45105=CARTESIAN_POINT('Ctrl Pts',(-85.8278893264213,-4.36795958291779,
1.23195236353769));
#45106=CARTESIAN_POINT('Ctrl Pts',(-85.7093572271712,-4.42738680209512,
-0.997508721096433));
#45107=CARTESIAN_POINT('Ctrl Pts',(-85.5908251279211,-3.41762019713068,
-2.9860759756232));
#45108=CARTESIAN_POINT('Ctrl Pts',(-85.472293028671,-1.58251382146784,-4.25351943088223));
#45109=CARTESIAN_POINT('Ctrl Pts',(-85.3537609294211,0.63476246167444,-4.49375724325186));
#45110=CARTESIAN_POINT('Ctrl Pts',(-85.2352288301708,2.69874649045617,-3.64877307108568));
#45111=CARTESIAN_POINT('Ctrl Pts',(-85.1166967309209,4.11099548692616,-1.92262675798041));
#45112=CARTESIAN_POINT('Ctrl Pts',(-84.9981646316706,4.53045772629236,0.267825193563669));
#45113=CARTESIAN_POINT('Ctrl Pts',(-84.8796325324207,3.8558349809911,2.39359857607639));
#45114=CARTESIAN_POINT('Ctrl Pts',(-84.7611004331704,2.2500455830191,3.94132876303992));
#45115=CARTESIAN_POINT('Ctrl Pts',(-84.6425683339206,0.100880385972347,
4.53724593688237));
#45116=CARTESIAN_POINT('Ctrl Pts',(-84.5240362346703,-2.072646966558,4.0374388040003));
#45117=CARTESIAN_POINT('Ctrl Pts',(-84.4055041354203,-3.74563948097091,
2.56260851918929));
#45118=CARTESIAN_POINT('Ctrl Pts',(-84.2869720361702,-4.51407705597339,
0.46891990442305));
#45119=CARTESIAN_POINT('Ctrl Pts',(-84.1684399369201,-4.19238550386574,
-1.73801073961178));
#45120=CARTESIAN_POINT('Ctrl Pts',(-84.0499078376701,-2.85825187485767,
-3.52521967597796));
#45121=CARTESIAN_POINT('Ctrl Pts',(-83.9313757384199,-0.833863386935234,
-4.46110405571966));
#45122=CARTESIAN_POINT('Ctrl Pts',(-83.8128436391699,1.39189932540943,-4.31965204755595));
#45123=CARTESIAN_POINT('Ctrl Pts',(-83.6943115399198,3.28152466618975,-3.13502366964235));
#45124=CARTESIAN_POINT('Ctrl Pts',(-83.5757794406697,4.37867668948207,-1.19330130018193));
#45125=CARTESIAN_POINT('Ctrl Pts',(-83.4572473414196,4.41839815981427,1.03659791885736));
#45126=CARTESIAN_POINT('Ctrl Pts',(-83.3387152421695,3.39109652233098,3.01616344389097));
#45127=CARTESIAN_POINT('Ctrl Pts',(-83.2201831429194,1.54486046126646,4.26733918258733));
#45128=CARTESIAN_POINT('Ctrl Pts',(-83.1016510436694,-0.674452391635007,
4.4879718710624));
#45129=CARTESIAN_POINT('Ctrl Pts',(-82.9831189444192,-2.73088805217719,
3.62477971613523));
#45130=CARTESIAN_POINT('Ctrl Pts',(-82.8645868451691,-4.12782663908925,
1.88621970662346));
#45131=CARTESIAN_POINT('Ctrl Pts',(-82.7460547459191,-4.5279138220188,-0.307853803615623));
#45132=CARTESIAN_POINT('Ctrl Pts',(-82.627522646669,-3.8345303616204,-2.42758201711926));
#45133=CARTESIAN_POINT('Ctrl Pts',(-82.5089905474189,-2.21512521746297,
-3.96106018825632));
#45134=CARTESIAN_POINT('Ctrl Pts',(-82.3904584481687,-0.0607773840669588,
-4.53796029661075));
#45135=CARTESIAN_POINT('Ctrl Pts',(-82.2719263489188,2.10824791181349,-4.01896358360754));
#45136=CARTESIAN_POINT('Ctrl Pts',(-82.1533942496687,3.76814090283094,-2.52940540057184));
#45137=CARTESIAN_POINT('Ctrl Pts',(-82.0348621504185,4.51804496315537,-0.429007290073176));
#45138=CARTESIAN_POINT('Ctrl Pts',(-81.9163300511686,4.17686166478898,1.77499413442573));
#45139=CARTESIAN_POINT('Ctrl Pts',(-81.7977979519183,2.82698522622225,3.5503425292147));
#45140=CARTESIAN_POINT('Ctrl Pts',(-81.6792658526684,0.794404682519185,
4.46829931231348));
#45141=CARTESIAN_POINT('Ctrl Pts',(-81.5607337534181,-1.43002098752725,
4.30718208568678));
#45142=CARTESIAN_POINT('Ctrl Pts',(-81.4422016541682,-3.30910307757889,
3.10589992852112));
#45143=CARTESIAN_POINT('Ctrl Pts',(-81.323669554918,-4.38905178892469,1.15455703114506));
#45144=CARTESIAN_POINT('Ctrl Pts',(-81.205137455668,-4.40906440787034,-1.07560615063343));
#45145=CARTESIAN_POINT('Ctrl Pts',(-81.0866053564178,-3.36430797774455,
-3.04601532742597));
#45146=CARTESIAN_POINT('Ctrl Pts',(-80.9680732571678,-1.50708643600638,
-4.28082562345572));
#45147=CARTESIAN_POINT('Ctrl Pts',(-80.8495411579177,0.714089641862045,
-4.48183595498707));
#45148=CARTESIAN_POINT('Ctrl Pts',(-80.7310090586676,2.76281631128911,-3.60050323900763));
#45149=CARTESIAN_POINT('Ctrl Pts',(-80.6124769594176,4.14433537737989,-1.84966532751926));
#45150=CARTESIAN_POINT('Ctrl Pts',(-80.4939448601674,4.52501625409684,0.34785836800249));
#45151=CARTESIAN_POINT('Ctrl Pts',(-80.3754127609173,3.81292623699154,2.46137584600368));
#45152=CARTESIAN_POINT('Ctrl Pts',(-80.2568806616673,2.18003183420017,3.98048222529689));
#45153=CARTESIAN_POINT('Ctrl Pts',(-80.1383485624171,0.0206696349967715,
4.53832020798643));
#45154=CARTESIAN_POINT('Ctrl Pts',(-80.0198164631671,-2.1436841872716,4.00017445235445));
#45155=CARTESIAN_POINT('Ctrl Pts',(-79.901284363917,-3.79034800494341,2.49600471663431));
#45156=CARTESIAN_POINT('Ctrl Pts',(-79.7827522646669,-4.52165997751698,
0.38906116707308));
#45157=CARTESIAN_POINT('Ctrl Pts',(-79.6642201654169,-4.16101158184665,
-1.8118388890356));
#45158=CARTESIAN_POINT('Ctrl Pts',(-79.5456880661666,-2.79549776906375,
-3.5751880743682));
#45159=CARTESIAN_POINT('Ctrl Pts',(-79.4271559669167,-0.754883929230383,
-4.47514556159899));
#45160=CARTESIAN_POINT('Ctrl Pts',(-79.3086238676665,1.46803095444983,-4.29437570094498));
#45161=CARTESIAN_POINT('Ctrl Pts',(-79.1900917684164,3.33642302337897,-3.07653359360171));
#45162=CARTESIAN_POINT('Ctrl Pts',(-79.0715596691664,4.39908407107168,-1.11572258260244));
#45163=CARTESIAN_POINT('Ctrl Pts',(-78.9530275699163,4.39938627489934,1.11453036951301));
#45164=CARTESIAN_POINT('Ctrl Pts',(-78.8344954706662,3.3372566565595,3.07562929473458));
#45165=CARTESIAN_POINT('Ctrl Pts',(-78.7159633714162,1.46919469449974,4.29397769977425));
#45166=CARTESIAN_POINT('Ctrl Pts',(-78.5974312721659,-0.753671113130901,
4.47534997493514));
#45167=CARTESIAN_POINT('Ctrl Pts',(-78.478899172916,-2.79452878052665,3.57594553456924));
#45168=CARTESIAN_POINT('Ctrl Pts',(-78.3603670736658,-4.16052039911434,
1.81296647846714));
#45169=CARTESIAN_POINT('Ctrl Pts',(-78.2418349744158,-4.52176527549064,
-0.387835767370506));
#45170=CARTESIAN_POINT('Ctrl Pts',(-78.1233028751657,-3.79102424088914,
-2.49497741250814));
#45171=CARTESIAN_POINT('Ctrl Pts',(-78.0047707759156,-2.14476828234976,
-3.99959337865132));
#45172=CARTESIAN_POINT('Ctrl Pts',(-77.8862386766655,0.0194399461672552,
-4.53832559960748));
#45173=CARTESIAN_POINT('Ctrl Pts',(-77.7677065774155,2.17895258677039,-3.98107296499709));
#45174=CARTESIAN_POINT('Ctrl Pts',(-77.6491744781653,3.81225993554848,-2.46240890062791));
#45175=CARTESIAN_POINT('Ctrl Pts',(-77.5306423789153,4.52492003879919,-0.349085009145456));
#45176=CARTESIAN_POINT('Ctrl Pts',(-77.4121102796651,4.14484007370081,1.84854283780517));
#45177=CARTESIAN_POINT('Ctrl Pts',(-77.2935781804151,2.76378475142464,3.59975293643636));
#45178=CARTESIAN_POINT('Ctrl Pts',(-77.175046081165,0.715318737465615,4.48164515764665));
#45179=CARTESIAN_POINT('Ctrl Pts',(-77.056513981915,-1.5059555074119,4.28122807559381));
#45180=CARTESIAN_POINT('Ctrl Pts',(-76.9379818826647,-3.36342346061332,
3.04693867596547));
#45181=CARTESIAN_POINT('Ctrl Pts',(-76.8194497834148,-4.40889139399587,
1.07677738930539));
#45182=CARTESIAN_POINT('Ctrl Pts',(-76.7009176841647,-4.3891255751704,-1.15332000830917));
#45183=CARTESIAN_POINT('Ctrl Pts',(-76.5823855849146,-3.31042589237266,
-3.10509875112957));
#45184=CARTESIAN_POINT('Ctrl Pts',(-76.4638534856645,-1.43021906913979,
-4.30660160725856));
#45185=CARTESIAN_POINT('Ctrl Pts',(-76.3453213864143,0.791242483179356,
-4.46890271793249));
#45186=CARTESIAN_POINT('Ctrl Pts',(-76.2267892871643,2.82994415375967,-3.55032611690991));
#45187=CARTESIAN_POINT('Ctrl Pts',(-76.1082571879142,4.16858782107412,-1.77770875490129));
#45188=CARTESIAN_POINT('Ctrl Pts',(-75.9502143889141,4.65283959303529,1.16727647387843));
#45189=CARTESIAN_POINT('Ctrl Pts',(-75.752660890164,2.39463673037035,4.54809328417136));
#45190=CARTESIAN_POINT('Ctrl Pts',(-75.5155966916638,-2.51039039858494,
4.48820167495918));
#45191=CARTESIAN_POINT('Ctrl Pts',(-75.2785324931636,-5.12648204836021,
0.349307700817715));
#45192=CARTESIAN_POINT('Ctrl Pts',(-75.0414682946634,-3.09472277798867,
-4.10400990228395));
#45193=CARTESIAN_POINT('Ctrl Pts',(-74.8044040961632,1.74869629074469,-4.83359106352794));
#45194=CARTESIAN_POINT('Ctrl Pts',(-74.5673398976631,5.0035277357217,-1.1753008420958));
#45195=CARTESIAN_POINT('Ctrl Pts',(-74.3302756991629,3.71748866958139,3.54959794684745));
#45196=CARTESIAN_POINT('Ctrl Pts',(-74.0932115006628,-0.942978294709073,
5.05246611144249));
#45197=CARTESIAN_POINT('Ctrl Pts',(-73.8561473021625,-4.74767723665014,
1.97005130473179));
#45198=CARTESIAN_POINT('Ctrl Pts',(-73.6190831036625,-4.24254907628667,
-2.90189312104113));
#45199=CARTESIAN_POINT('Ctrl Pts',(-73.3820189051621,0.112188250344633,
-5.13714393982636));
#45200=CARTESIAN_POINT('Ctrl Pts',(-73.1449547066621,4.36748045052756,-2.7149822729943));
#45201=CARTESIAN_POINT('Ctrl Pts',(-72.9078905081619,4.65382788827805,2.1820457323917));
#45202=CARTESIAN_POINT('Ctrl Pts',(-72.7103370094117,1.3809045066915,4.5939692411232));
#45203=CARTESIAN_POINT('Ctrl Pts',(-72.5522942104116,-1.58330196202896,
4.24623689121268));
#45204=CARTESIAN_POINT('Ctrl Pts',(-72.4337621111616,-3.41584817302406,
2.99088293128623));
#45205=CARTESIAN_POINT('Ctrl Pts',(-72.3152300119113,-4.42759428865317,
0.996777299409477));
#45206=CARTESIAN_POINT('Ctrl Pts',(-72.1966979126615,-4.36805595937351,
-1.22980938569953));
#45207=CARTESIAN_POINT('Ctrl Pts',(-72.0781658134112,-3.25466509626123,
-3.16349695026509));
#45208=CARTESIAN_POINT('Ctrl Pts',(-71.9596337141612,-1.35478431843691,
-4.33118110989355));
#45209=CARTESIAN_POINT('Ctrl Pts',(-71.8411016149111,0.872020940484935,
-4.45391427280835));
#45210=CARTESIAN_POINT('Ctrl Pts',(-71.722569515661,2.88836112437056,-3.50054605536382));
#45211=CARTESIAN_POINT('Ctrl Pts',(-71.6040374164109,4.20711361992387,-1.70206075526345));
#45212=CARTESIAN_POINT('Ctrl Pts',(-71.4855053171608,4.50989784278735,0.507588083832879));
#45213=CARTESIAN_POINT('Ctrl Pts',(-71.3669732179108,3.72354701697782,2.59459533799494));
#45214=CARTESIAN_POINT('Ctrl Pts',(-71.2484411186606,2.03798402017123,4.05505006051512));
#45215=CARTESIAN_POINT('Ctrl Pts',(-71.1299090194107,-0.139746613614768,
4.53621346335462));
#45216=CARTESIAN_POINT('Ctrl Pts',(-71.0113769201604,-2.28372721571331,
3.92190940924059));
#45217=CARTESIAN_POINT('Ctrl Pts',(-70.8928448209104,-3.87619898010495,
2.36047829785777));
#45218=CARTESIAN_POINT('Ctrl Pts',(-70.7743127216604,-4.53258582022182,
0.229004239881362));
#45219=CARTESIAN_POINT('Ctrl Pts',(-70.6557806224101,-4.09437397816109,
-1.9577742225503));
#45220=CARTESIAN_POINT('Ctrl Pts',(-70.5372485231602,-2.66738928497651,
-3.67175863671992));
#45221=CARTESIAN_POINT('Ctrl Pts',(-70.41871642391,-0.596242238417822,-4.49903022686127));
#45222=CARTESIAN_POINT('Ctrl Pts',(-70.30018432466,1.61889463121599,-4.23980631827825));
#45223=CARTESIAN_POINT('Ctrl Pts',(-70.1816522254098,3.44307577905915,-2.95668847717401));
#45224=CARTESIAN_POINT('Ctrl Pts',(-70.0631201261598,4.43576975553545,-0.95954375658275));
#45225=CARTESIAN_POINT('Ctrl Pts',(-69.9445880269097,4.35724545924099,1.26932641366537));
#45226=CARTESIAN_POINT('Ctrl Pts',(-69.8260559276596,3.22646615654172,3.19166002122267));
#45227=CARTESIAN_POINT('Ctrl Pts',(-69.7075238284095,1.31650991577464,4.34322221190749));
#45228=CARTESIAN_POINT('Ctrl Pts',(-69.5889917291594,-0.911377495780072,
4.44591594678435));
#45229=CARTESIAN_POINT('Ctrl Pts',(-69.4704596299094,-2.91917137754172,
3.47494115231241));
#45230=CARTESIAN_POINT('Ctrl Pts',(-69.3519275306593,-4.22199861680048,
1.66478383696633));
#45231=CARTESIAN_POINT('Ctrl Pts',(-69.2333954314092,-4.50523234680097,
-0.547411221521476));
#45232=CARTESIAN_POINT('Ctrl Pts',(-69.1148633321591,-3.70047290679963,
-2.62740895370075));
#45233=CARTESIAN_POINT('Ctrl Pts',(-68.996331232909,-2.00206605012669,-4.0728993450629));
#45234=CARTESIAN_POINT('Ctrl Pts',(-68.8777991336589,0.179830673601517,
-4.53480302470077));
#45235=CARTESIAN_POINT('Ctrl Pts',(-68.7592670344089,2.31829910560496,-3.90157234983416));
#45236=CARTESIAN_POINT('Ctrl Pts',(-68.6407349351587,3.89690882252018,-2.32612965524106));
#45237=CARTESIAN_POINT('Ctrl Pts',(-68.5222028359087,4.53443274040068,-0.188937203354069));
#45238=CARTESIAN_POINT('Ctrl Pts',(-68.4036707366585,4.07691172574293,1.99388272587192));
#45239=CARTESIAN_POINT('Ctrl Pts',(-68.2851386374085,2.63483502765729,3.69518902372516));
#45240=CARTESIAN_POINT('Ctrl Pts',(-68.1666065381584,0.556457625537843,
4.50412393868227));
#45241=CARTESIAN_POINT('Ctrl Pts',(-68.0480744389084,-1.65630176831098,
4.2253333591942));
#45242=CARTESIAN_POINT('Ctrl Pts',(-67.9295423396582,-3.46907180031879,
2.92614394523961));
#45243=CARTESIAN_POINT('Ctrl Pts',(-67.8110102404082,-4.44407673291178,
0.920304045422876));
#45244=CARTESIAN_POINT('Ctrl Pts',(-67.692478141158,-4.34585729879867,-1.30778510563007));
#45245=CARTESIAN_POINT('Ctrl Pts',(-67.573946041908,-3.19813304566272,-3.22005008754051));
#45246=CARTESIAN_POINT('Ctrl Pts',(-67.4554139426579,-1.2780741730198,-4.35468758377558));
#45247=CARTESIAN_POINT('Ctrl Pts',(-67.3368818434078,0.950633813348891,
-4.43768778723192));
#45248=CARTESIAN_POINT('Ctrl Pts',(-67.2183497441577,2.94976804714372,-3.44900652537501));
#45249=CARTESIAN_POINT('Ctrl Pts',(-67.0998176449076,4.2365466816572,-1.6274058369592));
#45250=CARTESIAN_POINT('Ctrl Pts',(-66.9812855456576,4.50021851520795,0.587205976986872));
#45251=CARTESIAN_POINT('Ctrl Pts',(-66.8627534464074,3.67710799636248,2.66001021184443));
#45252=CARTESIAN_POINT('Ctrl Pts',(-66.7442213471574,1.9659925806888,4.09043404991525));
#45253=CARTESIAN_POINT('Ctrl Pts',(-66.6256892479072,-0.219901122842242,
4.53303662462618));
#45254=CARTESIAN_POINT('Ctrl Pts',(-66.5071571486572,-2.35268970297329,
3.88093142242336));
#45255=CARTESIAN_POINT('Ctrl Pts',(-66.3886250494071,-3.91731439479203,
2.29159889081503));
#45256=CARTESIAN_POINT('Ctrl Pts',(-66.270092950157,-4.53592543446018,0.14885562484077));
#45257=CARTESIAN_POINT('Ctrl Pts',(-66.1515608509069,-4.05913106274721,
-2.0298355991238));
#45258=CARTESIAN_POINT('Ctrl Pts',(-66.0330287516569,-2.60207495704307,
-3.7183307359565));
#45259=CARTESIAN_POINT('Ctrl Pts',(-65.9144966524067,-0.516629555714746,
-4.50886587139066));
#45260=CARTESIAN_POINT('Ctrl Pts',(-65.7959645531567,1.69357953919417,-4.21053035714652));
#45261=CARTESIAN_POINT('Ctrl Pts',(-65.6774324539066,3.49479685973577,-2.89537086626402));
#45262=CARTESIAN_POINT('Ctrl Pts',(-65.5589003546564,4.4520365957367,-0.880992448464069));
#45263=CARTESIAN_POINT('Ctrl Pts',(-65.4403682554065,4.33412969427594,1.3461416482767));
#45264=CARTESIAN_POINT('Ctrl Pts',(-65.3218361561563,3.16955013707242,3.2481886448625));
#45265=CARTESIAN_POINT('Ctrl Pts',(-65.2033040569063,1.2395386030961,4.36581282185392));
#45266=CARTESIAN_POINT('Ctrl Pts',(-65.0847719576561,-0.989815879318478,
4.42911301154967));
#45267=CARTESIAN_POINT('Ctrl Pts',(-64.966239858406,-2.98013431800993,3.42280250535274));
#45268=CARTESIAN_POINT('Ctrl Pts',(-64.847707759156,-4.25076384078795,1.58990072453571));
#45269=CARTESIAN_POINT('Ctrl Pts',(-64.7291756599058,-4.49485318318126,
-0.626954867334768));
#45270=CARTESIAN_POINT('Ctrl Pts',(-64.6106435606558,-3.6534558765185,-2.692403703452));
#45271=CARTESIAN_POINT('Ctrl Pts',(-64.4921114614057,-1.92976555265208,
-4.10764926153961));
#45272=CARTESIAN_POINT('Ctrl Pts',(-64.3735793621557,0.259954396175193,
-4.53091616077132));
#45273=CARTESIAN_POINT('Ctrl Pts',(-64.2550472629055,2.38689653782794,-3.85998736548898));
#45274=CARTESIAN_POINT('Ctrl Pts',(-64.1365151636555,3.93741399575905,-2.25688913552044));
#45275=CARTESIAN_POINT('Ctrl Pts',(-64.0179830644053,4.5370638391048,-0.108762419599618));
#45276=CARTESIAN_POINT('Ctrl Pts',(-63.8994509651554,4.04103335151306,2.06562992716232));
#45277=CARTESIAN_POINT('Ctrl Pts',(-63.7809188659052,2.56911164507772,3.74118201898217));
#45278=CARTESIAN_POINT('Ctrl Pts',(-63.6623867666552,0.476761133292039,
4.51325562823685));
#45279=CARTESIAN_POINT('Ctrl Pts',(-63.543854667405,-1.73072502895579,4.19539848145269));
#45280=CARTESIAN_POINT('Ctrl Pts',(-63.425322568155,-3.52024894960062,2.86437163735175));
#45281=CARTESIAN_POINT('Ctrl Pts',(-63.3067904689048,-4.45964872148725,
0.841612039461598));
#45282=CARTESIAN_POINT('Ctrl Pts',(-63.1882583696549,-4.32206356208222,
-1.38439304727765));
#45283=CARTESIAN_POINT('Ctrl Pts',(-63.0697262704046,-3.14071966311106,
-3.27607349456283));
#45284=CARTESIAN_POINT('Ctrl Pts',(-62.9511941711547,-1.20090621601503,
-4.37659705757406));
#45285=CARTESIAN_POINT('Ctrl Pts',(-62.8326620719044,1.02892063332738,-4.42019228929496));
#45286=CARTESIAN_POINT('Ctrl Pts',(-62.7141299726545,3.01026781828531,-3.39633113907137));
#45287=CARTESIAN_POINT('Ctrl Pts',(-62.5955978734043,4.26464898373894,-1.55227142907499));
#45288=CARTESIAN_POINT('Ctrl Pts',(-62.4770657741543,4.48913676978754,0.666654787858014));
#45289=CARTESIAN_POINT('Ctrl Pts',(-62.3585336749041,3.62951839467588,2.72458689836349));
#45290=CARTESIAN_POINT('Ctrl Pts',(-62.2400015756541,1.89338779561597,4.12454363529436));
#45291=CARTESIAN_POINT('Ctrl Pts',(-62.1214694764039,-0.29998736514476,
4.52844179876308));
#45292=CARTESIAN_POINT('Ctrl Pts',(-62.002937377154,-2.42091693835619,3.83874181491576));
#45293=CARTESIAN_POINT('Ctrl Pts',(-61.8844052779038,-3.95720605550443,
2.22200310044728));
#45294=CARTESIAN_POINT('Ctrl Pts',(-61.7658731786537,-4.53784786539412,
0.0686607192070461));
#45295=CARTESIAN_POINT('Ctrl Pts',(-61.6473410794036,-4.02262000565155,
-2.10126291418506));
#45296=CARTESIAN_POINT('Ctrl Pts',(-61.5288089801535,-2.53594766634852,
-3.76374108794713));
#45297=CARTESIAN_POINT('Ctrl Pts',(-61.4102768809035,-0.436855472474266,
-4.51729286634914));
#45298=CARTESIAN_POINT('Ctrl Pts',(-61.2917447816534,1.76773533663033,-4.1799389140226));
#45299=CARTESIAN_POINT('Ctrl Pts',(-61.1732126824033,3.54542608116568,-2.83314867977618));
#45300=CARTESIAN_POINT('Ctrl Pts',(-61.0546805831532,4.46691251711184,-0.802165894310029));
#45301=CARTESIAN_POINT('Ctrl Pts',(-60.9361484839031,4.30965984162703,1.42253631489993));
#45302=CARTESIAN_POINT('Ctrl Pts',(-60.817616384653,3.11164388178486,3.30370245865813));
#45303=CARTESIAN_POINT('Ctrl Pts',(-60.6990842854029,1.16218001690214,4.38703944854634));
#45304=CARTESIAN_POINT('Ctrl Pts',(-60.5805521861529,-1.06794499613072,
4.41092631736494));
#45305=CARTESIAN_POINT('Ctrl Pts',(-60.4620200869028,-3.04016624441482,
3.36959449389407));
#45306=CARTESIAN_POINT('Ctrl Pts',(-60.3434879876527,-4.27820092508761,
1.51452089020126));
#45307=CARTESIAN_POINT('Ctrl Pts',(-60.2249558884026,-4.48306992471128,
-0.706302638699686));
#45308=CARTESIAN_POINT('Ctrl Pts',(-60.1064237891525,-3.60529701130859,
-2.75655728081619));
#45309=CARTESIAN_POINT('Ctrl Pts',(-59.9878916899025,-1.85686297511547,
-4.14111585566494));
#45310=CARTESIAN_POINT('Ctrl Pts',(-59.8693595906524,0.339998562725392,
-4.52561372368815));
#45311=CARTESIAN_POINT('Ctrl Pts',(-59.7508274914022,2.45474490441493,-3.81719644661123));
#45312=CARTESIAN_POINT('Ctrl Pts',(-59.6322953921522,3.97669576066936,-2.18694347728569));
#45313=CARTESIAN_POINT('Ctrl Pts',(-59.513763292902,4.53826389257849,-0.0285537226009381));
#45314=CARTESIAN_POINT('Ctrl Pts',(-59.395231193652,4.00391977626628,2.1367319098308));
#45315=CARTESIAN_POINT('Ctrl Pts',(-59.2766990944019,2.50253054516668,3.78600593266119));
#45316=CARTESIAN_POINT('Ctrl Pts',(-59.1581669951518,0.397027511556691,
4.52097743498945));
#45317=CARTESIAN_POINT('Ctrl Pts',(-59.0396348959017,-1.80484254084631,
4.16415511545482));
#45318=CARTESIAN_POINT('Ctrl Pts',(-58.9606134964017,-2.98134669247437,
3.25577591290924));
#45319=CARTESIAN_POINT('Ctrl Pts',(-58.9211027966516,-3.42633377868327,
2.68871070989395));
#45320=CARTESIAN_POINT('Ctrl Pts',(-89.575,2.36230756092335,-3.31488661006744));
#45321=CARTESIAN_POINT('Ctrl Pts',(-89.53548930025,2.91092803106123,-2.9239199082961));
#45322=CARTESIAN_POINT('Ctrl Pts',(-89.4564679007499,3.80977362498712,-1.86473730182378));
#45323=CARTESIAN_POINT('Ctrl Pts',(-89.3379358014998,4.23793920928767,0.175536844418832));
#45324=CARTESIAN_POINT('Ctrl Pts',(-89.2194037022498,3.6426422996848,2.17296520226056));
#45325=CARTESIAN_POINT('Ctrl Pts',(-89.1008716029996,2.16767467238955,3.64585259348834));
#45326=CARTESIAN_POINT('Ctrl Pts',(-88.9823395037495,0.169217900166083,
4.23817423904527));
#45327=CARTESIAN_POINT('Ctrl Pts',(-88.8638074044995,-1.87010146406577,
3.80705007020246));
#45328=CARTESIAN_POINT('Ctrl Pts',(-88.7452753052494,-3.45780118263798,
2.45651375596413));
#45329=CARTESIAN_POINT('Ctrl Pts',(-88.6267432059994,-4.21045692323235,
0.512753836099102));
#45330=CARTESIAN_POINT('Ctrl Pts',(-88.5082111067491,-3.94630675958036,
-1.5548404226029));
#45331=CARTESIAN_POINT('Ctrl Pts',(-88.3896790074992,-2.72914125118652,
-3.24694449006369));
#45332=CARTESIAN_POINT('Ctrl Pts',(-88.271146908249,-0.852900597114338,
-4.15492782628333));
#45333=CARTESIAN_POINT('Ctrl Pts',(-88.152614808999,1.22931172268961,-4.05951413513238));
#45334=CARTESIAN_POINT('Ctrl Pts',(-88.0340827097489,3.01465081869963,-2.98374660176146));
#45335=CARTESIAN_POINT('Ctrl Pts',(-87.9155506104989,4.07196543070694,-1.18741760272948));
#45336=CARTESIAN_POINT('Ctrl Pts',(-87.7970185112487,4.1459188620231,0.895667260529816));
#45337=CARTESIAN_POINT('Ctrl Pts',(-87.6784864119986,3.21865170212703,2.76245259353163));
#45338=CARTESIAN_POINT('Ctrl Pts',(-87.5599543127485,1.51409475903765,3.96211813494982));
#45339=CARTESIAN_POINT('Ctrl Pts',(-87.4414222134985,-0.556109197774073,
4.20495013639211));
#45340=CARTESIAN_POINT('Ctrl Pts',(-87.3228901142483,-2.49201530688875,
3.43230575316451));
#45341=CARTESIAN_POINT('Ctrl Pts',(-87.2043580149983,-3.82611102636026,
1.830775107081));
#45342=CARTESIAN_POINT('Ctrl Pts',(-87.0858259157481,-4.23621829341267,
-0.212879421996658));
#45343=CARTESIAN_POINT('Ctrl Pts',(-86.9672938164981,-3.62329806373565,
-2.2051245358312));
#45344=CARTESIAN_POINT('Ctrl Pts',(-86.848761717248,-2.1353677918245,-3.66484208003093));
#45345=CARTESIAN_POINT('Ctrl Pts',(-86.730229617998,-0.131755887070526,
-4.23951689036003));
#45346=CARTESIAN_POINT('Ctrl Pts',(-86.6116975187478,1.90367446658495,-3.7903676078918));
#45347=CARTESIAN_POINT('Ctrl Pts',(-86.4931654194978,3.47937607418291,-2.42586174626368));
#45348=CARTESIAN_POINT('Ctrl Pts',(-86.3746333202476,4.21482414698068,-0.475521279897397));
#45349=CARTESIAN_POINT('Ctrl Pts',(-86.2561012209977,3.93241131237811,1.58965541797289));
#45350=CARTESIAN_POINT('Ctrl Pts',(-86.1375691217474,2.70033898852751,3.27093754520615));
#45351=CARTESIAN_POINT('Ctrl Pts',(-86.0190370224974,0.816147051306786,
4.16230309663427));
#45352=CARTESIAN_POINT('Ctrl Pts',(-85.9005049232474,-1.26514069566702,
4.04849133601287));
#45353=CARTESIAN_POINT('Ctrl Pts',(-85.7819728239972,-3.04090270501211,
2.95698728713125));
#45354=CARTESIAN_POINT('Ctrl Pts',(-85.6634407247472,-4.08230050870968,
1.15138422526712));
#45355=CARTESIAN_POINT('Ctrl Pts',(-85.544908625497,-4.13784126234383,-0.932272902775868));
#45356=CARTESIAN_POINT('Ctrl Pts',(-85.426376526247,-3.19411212591926,-2.79079035483874));
#45357=CARTESIAN_POINT('Ctrl Pts',(-85.3078444269969,-1.47901940386148,
-3.97534459897585));
#45358=CARTESIAN_POINT('Ctrl Pts',(-85.1893123277468,0.593249793413271,
-4.19987115995485));
#45359=CARTESIAN_POINT('Ctrl Pts',(-85.0707802284967,2.52225185735541,-3.41014789205285));
#45360=CARTESIAN_POINT('Ctrl Pts',(-84.9522481292466,3.84214154206329,-1.79688938122436));
#45361=CARTESIAN_POINT('Ctrl Pts',(-84.8337160299966,4.23417147746969,0.250309762069736));
#45362=CARTESIAN_POINT('Ctrl Pts',(-84.7151839307464,3.60366821294754,2.23706023356476));
#45363=CARTESIAN_POINT('Ctrl Pts',(-84.5966518314964,2.10289542607052,3.6835708089593));
#45364=CARTESIAN_POINT('Ctrl Pts',(-84.4781197322463,0.094282935351365,
4.24051574760746));
#45365=CARTESIAN_POINT('Ctrl Pts',(-84.3595876329963,-1.9370984564613,3.77339537387491));
#45366=CARTESIAN_POINT('Ctrl Pts',(-84.241055533746,-3.50067936031506,2.39501713853357));
#45367=CARTESIAN_POINT('Ctrl Pts',(-84.1225234344961,-4.21886208242914,
0.43825313124611));
#45368=CARTESIAN_POINT('Ctrl Pts',(-84.0039913352459,-3.91820875405299,
-1.62434701873333));
#45369=CARTESIAN_POINT('Ctrl Pts',(-83.8854592359959,-2.67132578982276,
-3.29467473390518));
#45370=CARTESIAN_POINT('Ctrl Pts',(-83.7669271367457,-0.779329768066677,
-4.16935344990209));
#45371=CARTESIAN_POINT('Ctrl Pts',(-83.6483950374957,1.3008708565925,-4.03715222552651));
#45372=CARTESIAN_POINT('Ctrl Pts',(-83.5298629382456,3.06691707187941,-2.92999705662308));
#45373=CARTESIAN_POINT('Ctrl Pts',(-83.4113308389955,4.0923167299564,-1.11526089294132));
#45374=CARTESIAN_POINT('Ctrl Pts',(-83.2927987397454,4.12944046598591,0.968805716066663));
#45375=CARTESIAN_POINT('Ctrl Pts',(-83.1742666404953,3.16932306615985,2.81891014044657));
#45376=CARTESIAN_POINT('Ctrl Pts',(-83.0557345412452,1.44382852615606,3.98826055626553));
#45377=CARTESIAN_POINT('Ctrl Pts',(-82.9372024419952,-0.630344051771873,
4.19446414384497));
#45378=CARTESIAN_POINT('Ctrl Pts',(-82.818670342745,-2.55229140128288,3.38772367240052));
#45379=CARTESIAN_POINT('Ctrl Pts',(-82.700138243495,-3.8578719580008,1.76286330532926));
#45380=CARTESIAN_POINT('Ctrl Pts',(-82.581606144245,-4.23179394134261,-0.287720551266843));
#45381=CARTESIAN_POINT('Ctrl Pts',(-82.4630740449948,-3.58375688894285,
-2.26882120021829));
#45382=CARTESIAN_POINT('Ctrl Pts',(-82.3445419457447,-2.0702588085909,-3.70201182373276));
#45383=CARTESIAN_POINT('Ctrl Pts',(-82.2260098464947,-0.0568026194346637,
-4.24118338910624));
#45384=CARTESIAN_POINT('Ctrl Pts',(-82.1074777472446,1.97037114458219,-3.75612840970636));
#45385=CARTESIAN_POINT('Ctrl Pts',(-81.9889456479944,3.52170921742845,-2.36398546219828));
#45386=CARTESIAN_POINT('Ctrl Pts',(-81.8704135487444,4.2225704934618,-0.40095075177776));
#45387=CARTESIAN_POINT('Ctrl Pts',(-81.7518814494942,3.90370015456685,1.65891174594675));
#45388=CARTESIAN_POINT('Ctrl Pts',(-81.6333493502442,2.64210394076326,3.31815458407359));
#45389=CARTESIAN_POINT('Ctrl Pts',(-81.514817250994,0.742451613392211,4.17607814574591));
#45390=CARTESIAN_POINT('Ctrl Pts',(-81.3962851517442,-1.33649940985683,
4.02549778351171));
#45391=CARTESIAN_POINT('Ctrl Pts',(-81.2777530524938,-3.09269188977919,
2.90277797161605));
#45392=CARTESIAN_POINT('Ctrl Pts',(-81.159220953244,-4.10201331091795,1.07905045046897));
#45393=CARTESIAN_POINT('Ctrl Pts',(-81.0406888539936,-4.12071712970371,
-1.00526285844639));
#45394=CARTESIAN_POINT('Ctrl Pts',(-80.9221567547438,-3.14428645876529,
-2.84680974826745));
#45395=CARTESIAN_POINT('Ctrl Pts',(-80.8036246554935,-1.40852487473531,
-4.00086500082885));
#45396=CARTESIAN_POINT('Ctrl Pts',(-80.6850925562435,0.667389075585396,
-4.18872950897938));
#45397=CARTESIAN_POINT('Ctrl Pts',(-80.5665604569934,2.58213159232414,-3.36503484640604));
#45398=CARTESIAN_POINT('Ctrl Pts',(-80.4480283577433,3.87330104552845,-1.72869953673665));
#45399=CARTESIAN_POINT('Ctrl Pts',(-80.3294962584933,4.22908587072581,0.325108867355182));
#45400=CARTESIAN_POINT('Ctrl Pts',(-80.2109641592431,3.56356564694796,2.30040495511053));
#45401=CARTESIAN_POINT('Ctrl Pts',(-80.0924320599931,2.03746048854546,3.72016368392876));
#45402=CARTESIAN_POINT('Ctrl Pts',(-79.9738999607429,0.0193178668117769,
4.2415197627297));
#45403=CARTESIAN_POINT('Ctrl Pts',(-79.855367861493,-2.00348993210374,3.73856806405375));
#45404=CARTESIAN_POINT('Ctrl Pts',(-79.7368357622428,-3.54246400293638,
2.33276914106685));
#45405=CARTESIAN_POINT('Ctrl Pts',(-79.6183036629927,-4.2259490904216,0.36361705508285));
#45406=CARTESIAN_POINT('Ctrl Pts',(-79.4997715637427,-3.88888664715446,
-1.69334689985141));
#45407=CARTESIAN_POINT('Ctrl Pts',(-79.3812394644925,-2.61267572378093,
-3.34137526175934));
#45408=CARTESIAN_POINT('Ctrl Pts',(-79.2627073652425,-0.705515467763387,
-4.18247665892133));
#45409=CARTESIAN_POINT('Ctrl Pts',(-79.1441752659924,1.3720235726515,-4.01352892025788));
#45410=CARTESIAN_POINT('Ctrl Pts',(-79.0256431667423,3.11822514541502,-2.87533215814075));
#45411=CARTESIAN_POINT('Ctrl Pts',(-78.9071110674922,4.11138949440471,-1.04275572611736));
#45412=CARTESIAN_POINT('Ctrl Pts',(-78.7885789682421,4.11167193448134,1.04164148226761));
#45413=CARTESIAN_POINT('Ctrl Pts',(-78.670046868992,3.11900426003185,2.87448699928452));
#45414=CARTESIAN_POINT('Ctrl Pts',(-78.551514769742,1.37311120556277,4.01315694786418));
#45415=CARTESIAN_POINT('Ctrl Pts',(-78.4329826704918,-0.704381968314586,
4.18266770388186));
#45416=CARTESIAN_POINT('Ctrl Pts',(-78.3144505712418,-2.61177010587796,
3.34208318501393));
#45417=CARTESIAN_POINT('Ctrl Pts',(-78.1959184719917,-3.88842758715636,
1.69440074634939));
#45418=CARTESIAN_POINT('Ctrl Pts',(-78.0773863727416,-4.22604750203994,
-0.362471794982803));
#45419=CARTESIAN_POINT('Ctrl Pts',(-77.9588542734915,-3.54309601390001,
-2.33180902134115));
#45420=CARTESIAN_POINT('Ctrl Pts',(-77.8403221742414,-2.00450312872445,
-3.73802499184148));
#45421=CARTESIAN_POINT('Ctrl Pts',(-77.7217900749913,0.0181685980883059,
-4.2415248017455));
#45422=CARTESIAN_POINT('Ctrl Pts',(-77.6032579757413,2.03645182254301,-3.72071578999402));
#45423=CARTESIAN_POINT('Ctrl Pts',(-77.4847258764911,3.56294292078298,-2.30137044925895));
#45424=CARTESIAN_POINT('Ctrl Pts',(-77.3661937772411,4.22899594778787,-0.326255287706977));
#45425=CARTESIAN_POINT('Ctrl Pts',(-77.247661677991,3.87377273534343,1.72765045644101));
#45426=CARTESIAN_POINT('Ctrl Pts',(-77.1291295787409,2.58303669769032,3.36433361268123));
#45427=CARTESIAN_POINT('Ctrl Pts',(-77.0105974794908,0.668537789879148,
4.18855118954554));
#45428=CARTESIAN_POINT('Ctrl Pts',(-76.8920653802408,-1.40746790745146,
4.00124113310223));
#45429=CARTESIAN_POINT('Ctrl Pts',(-76.7735332809906,-3.14345978794428,
2.84767271097138));
#45430=CARTESIAN_POINT('Ctrl Pts',(-76.6550011817406,-4.12055543071948,
1.00635749957924));
#45431=CARTESIAN_POINT('Ctrl Pts',(-76.5364690824904,-4.1020822716358,-1.07789432737393));
#45432=CARTESIAN_POINT('Ctrl Pts',(-76.4179369832404,-3.09392819414575,
-2.90202919022035));
#45433=CARTESIAN_POINT('Ctrl Pts',(-76.2994048839903,-1.33668453718049,
-4.02495526764412));
#45434=CARTESIAN_POINT('Ctrl Pts',(-76.1808727847402,0.739496217920181,
-4.17664208939481));
#45435=CARTESIAN_POINT('Ctrl Pts',(-76.0623406854901,2.64486935815373,-3.3181392451129));
#45436=CARTESIAN_POINT('Ctrl Pts',(-75.9438085862401,3.89596740984592,-1.66144883365045));
#45437=CARTESIAN_POINT('Ctrl Pts',(-75.7857657872398,4.3485497237372,1.09093805761265));
#45438=CARTESIAN_POINT('Ctrl Pts',(-75.5882122884899,2.2380304938709,4.25065369199898));
#45439=CARTESIAN_POINT('Ctrl Pts',(-75.3511480899896,-2.34621401747439,
4.19467891885534));
#45440=CARTESIAN_POINT('Ctrl Pts',(-75.1140838914895,-4.79121655698383,
0.326463415623377));
#45441=CARTESIAN_POINT('Ctrl Pts',(-74.8770196929892,-2.89233179269924,
-3.83561280588861));
#45442=CARTESIAN_POINT('Ctrl Pts',(-74.639955494489,1.63433374823429,-4.51748027493275));
#45443=CARTESIAN_POINT('Ctrl Pts',(-74.402891295989,4.6763033020638,-1.09843764222045));
#45444=CARTESIAN_POINT('Ctrl Pts',(-74.1658270974887,3.47436957665643,3.31745869645859));
#45445=CARTESIAN_POINT('Ctrl Pts',(-73.9287628989886,-0.881308697829502,
4.72204116943823));
#45446=CARTESIAN_POINT('Ctrl Pts',(-73.6916987004883,-4.43718510449666,
1.84121242214388));
#45447=CARTESIAN_POINT('Ctrl Pts',(-73.4546345019883,-3.96509169180119,
-2.71211295328289));
#45448=CARTESIAN_POINT('Ctrl Pts',(-73.217570303488,0.104851279587011,-4.80118117413053));
#45449=CARTESIAN_POINT('Ctrl Pts',(-72.9805061049878,4.0818527109764,-2.5374258400941));
#45450=CARTESIAN_POINT('Ctrl Pts',(-72.7434419064878,4.34947338571156,2.0393426803231));
#45451=CARTESIAN_POINT('Ctrl Pts',(-72.5458884077375,1.29059508521834,4.29352941894811));
#45452=CARTESIAN_POINT('Ctrl Pts',(-72.3878456087375,-1.47975600101921,
3.96853832825987));
#45453=CARTESIAN_POINT('Ctrl Pts',(-72.2693135094873,-3.19245598996507,
2.7952829416349));
#45454=CARTESIAN_POINT('Ctrl Pts',(-72.1507814102373,-4.13803517954143,
0.931589315149122));
#45455=CARTESIAN_POINT('Ctrl Pts',(-72.0322493109872,-4.08239058226615,
-1.14938139548983));
#45456=CARTESIAN_POINT('Ctrl Pts',(-71.9137172117371,-3.04181408411095,
-2.95660822043184));
#45457=CARTESIAN_POINT('Ctrl Pts',(-71.7951851124869,-1.26618312449043,
-4.04792730165813));
#45458=CARTESIAN_POINT('Ctrl Pts',(-71.676653013237,0.814991865508356,-4.1626338697688));
#45459=CARTESIAN_POINT('Ctrl Pts',(-71.5581209139868,2.69946593220966,-3.27161473710967));
#45460=CARTESIAN_POINT('Ctrl Pts',(-71.4395888147368,3.93197366980717,-1.59074811823812));
#45461=CARTESIAN_POINT('Ctrl Pts',(-71.3210567154866,4.21495618453984,0.474392460257583));
#45462=CARTESIAN_POINT('Ctrl Pts',(-71.2025246162366,3.48003171573737,2.42491205953816));
#45463=CARTESIAN_POINT('Ctrl Pts',(-71.0839925169865,1.90470242326041,3.78985487631873));
#45464=CARTESIAN_POINT('Ctrl Pts',(-70.9654604177364,-0.130607360489598,
4.2395507965525));
#45465=CARTESIAN_POINT('Ctrl Pts',(-70.8469283184863,-2.13437432226263,
3.6654214565239));
#45466=CARTESIAN_POINT('Ctrl Pts',(-70.7283962192362,-3.62270043207957,
2.20610597997014));
#45467=CARTESIAN_POINT('Ctrl Pts',(-70.6098641199862,-4.2361603967273,0.214027650031447));
#45468=CARTESIAN_POINT('Ctrl Pts',(-70.491332020736,-3.82660705910867,-1.82973824572734));
#45469=CARTESIAN_POINT('Ctrl Pts',(-70.372799921486,-2.49294537375558,-3.43163023054535));
#45470=CARTESIAN_POINT('Ctrl Pts',(-70.2542678222358,-0.557248744408297,
-4.20479929705468));
#45471=CARTESIAN_POINT('Ctrl Pts',(-70.1357357229858,1.51302095431612,-3.96252830672392));
#45472=CARTESIAN_POINT('Ctrl Pts',(-70.0172036237356,3.21790294474063,-2.7633247619019));
#45473=CARTESIAN_POINT('Ctrl Pts',(-69.8986715244856,4.14567598115117,-0.896790799288985));
#45474=CARTESIAN_POINT('Ctrl Pts',(-69.7801394252355,4.07228707527332,1.18631405942714));
#45475=CARTESIAN_POINT('Ctrl Pts',(-69.6616073259855,3.01545931965475,2.98292946189813));
#45476=CARTESIAN_POINT('Ctrl Pts',(-69.5430752267353,1.23041181972154,4.05918093071395));
#45477=CARTESIAN_POINT('Ctrl Pts',(-69.4245431274853,-0.851774551486206,
4.15515862422754));
#45478=CARTESIAN_POINT('Ctrl Pts',(-69.3060110282352,-2.72826123349541,
3.24768436257942));
#45479=CARTESIAN_POINT('Ctrl Pts',(-69.1874789289851,-3.9458852065712,1.5559090636089));
#45480=CARTESIAN_POINT('Ctrl Pts',(-69.068946829735,-4.210595806135,-0.511611214725999));
#45481=CARTESIAN_POINT('Ctrl Pts',(-68.9504147304849,-3.45846662340299,
-2.45557970596334));
#45482=CARTESIAN_POINT('Ctrl Pts',(-68.8318826312348,-1.87113344337377,
-3.8065368400609));
#45483=CARTESIAN_POINT('Ctrl Pts',(-68.7133505319848,0.168069973265368,
-4.23823259881627));
#45484=CARTESIAN_POINT('Ctrl Pts',(-68.5948184327347,2.16668525394882,-3.64641441527627));
#45485=CARTESIAN_POINT('Ctrl Pts',(-68.4762863334845,3.64205587679515,-2.17400369546731));
#45486=CARTESIAN_POINT('Ctrl Pts',(-68.3577542342345,4.23788653064464,-0.176580947402252));
#45487=CARTESIAN_POINT('Ctrl Pts',(-68.2392221349844,3.81028681608063,1.86348529825389));
#45488=CARTESIAN_POINT('Ctrl Pts',(-68.1206900357343,2.46252012400403,3.45352829964948));
#45489=CARTESIAN_POINT('Ctrl Pts',(-68.0021579364842,0.520065995274375,
4.20955988651605));
#45490=CARTESIAN_POINT('Ctrl Pts',(-67.8836258372342,-1.54798171159727,
3.94900186099799));
#45491=CARTESIAN_POINT('Ctrl Pts',(-67.7650937379841,-3.24219885883922,
2.73477780401754));
#45492=CARTESIAN_POINT('Ctrl Pts',(-67.646561638734,-4.15343969263372,0.860117315986614));
#45493=CARTESIAN_POINT('Ctrl Pts',(-67.5280295394839,-4.0616436862299,-1.2222576012094));
#45494=CARTESIAN_POINT('Ctrl Pts',(-67.4094974402338,-2.98897915866447,
-3.00946285351303));
#45495=CARTESIAN_POINT('Ctrl Pts',(-67.2909653409837,-1.19448972629963,
-4.06989648165282));
#45496=CARTESIAN_POINT('Ctrl Pts',(-67.1724332417337,0.888463555159219,
-4.14746857598213));
#45497=CARTESIAN_POINT('Ctrl Pts',(-67.0539011424835,2.75685691930934,-3.22344582769147));
#45498=CARTESIAN_POINT('Ctrl Pts',(-66.9353690432335,3.95948184624652,-1.52097553788664));
#45499=CARTESIAN_POINT('Ctrl Pts',(-66.8168369439834,4.20590987283498,0.548803443132984));
#45500=CARTESIAN_POINT('Ctrl Pts',(-66.6983048447332,3.43662974878158,2.48604888274442));
#45501=CARTESIAN_POINT('Ctrl Pts',(-66.5797727454832,1.83741913355893,3.82292479722488));
#45502=CARTESIAN_POINT('Ctrl Pts',(-66.4612406462331,-0.205519865420819,
4.23658171908943));
#45503=CARTESIAN_POINT('Ctrl Pts',(-66.3427085469829,-2.19882674941518,
3.62712337861033));
#45504=CARTESIAN_POINT('Ctrl Pts',(-66.224176447733,-3.66112695025279,2.1417311996929));
#45505=CARTESIAN_POINT('Ctrl Pts',(-66.1056443484827,-4.23928160438623,
0.139120653814684));
#45506=CARTESIAN_POINT('Ctrl Pts',(-65.9871122492328,-3.79366898612715,
-1.89708689872192));
#45507=CARTESIAN_POINT('Ctrl Pts',(-65.8685801499826,-2.43190252088865,
-3.47515657294758));
#45508=CARTESIAN_POINT('Ctrl Pts',(-65.7500480507326,-0.482842631226866,
-4.21399170277722));
#45509=CARTESIAN_POINT('Ctrl Pts',(-65.6315159514825,1.58282156305449,-3.93516695670401));
#45510=CARTESIAN_POINT('Ctrl Pts',(-65.5129838522324,3.26624153165954,-2.70601724578163));
#45511=CARTESIAN_POINT('Ctrl Pts',(-65.3944517529823,4.16087899042085,-0.823376648126326));
#45512=CARTESIAN_POINT('Ctrl Pts',(-65.2759196537323,4.05068305232286,1.25810567411077));
#45513=CARTESIAN_POINT('Ctrl Pts',(-65.1573875544821,2.96226553641969,3.03576118450472));
#45514=CARTESIAN_POINT('Ctrl Pts',(-65.0388554552321,1.1584743342804,4.08029414312485));
#45515=CARTESIAN_POINT('Ctrl Pts',(-64.9203233559819,-0.925083163194395,
4.13945457986673));
#45516=CARTESIAN_POINT('Ctrl Pts',(-64.8017912567319,-2.78523727417561,
3.19895551768826));
#45517=CARTESIAN_POINT('Ctrl Pts',(-64.6832591574818,-3.97276922101502,
1.4859232127405));
#45518=CARTESIAN_POINT('Ctrl Pts',(-64.5647270582317,-4.20089542678846,
-0.585952805943586));
#45519=CARTESIAN_POINT('Ctrl Pts',(-64.4461949589816,-3.41452444788805,
-2.51632388066006));
#45520=CARTESIAN_POINT('Ctrl Pts',(-64.3276628597316,-1.80356130768488,
-3.83901415561695));
#45521=CARTESIAN_POINT('Ctrl Pts',(-64.2091307604814,0.242953704951307,
-4.23459993090915));
#45522=CARTESIAN_POINT('Ctrl Pts',(-64.0905986612314,2.23079650020559,-3.60754903671119));
#45523=CARTESIAN_POINT('Ctrl Pts',(-63.9720665619813,3.67991206254491,-2.10929141882807));
#45524=CARTESIAN_POINT('Ctrl Pts',(-63.8535344627312,4.24034555879598,-0.101649493872672));
#45525=CARTESIAN_POINT('Ctrl Pts',(-63.7350023634811,3.77675484249208,1.93054032263455));
#45526=CARTESIAN_POINT('Ctrl Pts',(-63.6164702642311,2.40109496815141,3.49651341074552));
#45527=CARTESIAN_POINT('Ctrl Pts',(-63.4979381649809,0.445581553589111,
4.21809437503554));
#45528=CARTESIAN_POINT('Ctrl Pts',(-63.3794060657309,-1.61753778440945,
3.92102468668754));
#45529=CARTESIAN_POINT('Ctrl Pts',(-63.2608739664807,-3.29002908679384,
2.67704532753104));
#45530=CARTESIAN_POINT('Ctrl Pts',(-63.1423418672307,-4.16799329270179,
0.786571668443664));
#45531=CARTESIAN_POINT('Ctrl Pts',(-63.0238097679806,-4.03940603002961,
-1.29385547962891));
#45532=CARTESIAN_POINT('Ctrl Pts',(-62.9052776687305,-2.93532053926837,
-3.06182240003477));
#45533=CARTESIAN_POINT('Ctrl Pts',(-62.7867455694804,-1.12236845682437,
-4.09037310336489));
#45534=CARTESIAN_POINT('Ctrl Pts',(-62.6682134702303,0.961630515374074,
-4.13111726165049));
#45535=CARTESIAN_POINT('Ctrl Pts',(-62.5496813709802,2.81340008135553,-3.17421534553572));
#45536=CARTESIAN_POINT('Ctrl Pts',(-62.4311492717302,3.98574629304517,-1.4507548259719));
#45537=CARTESIAN_POINT('Ctrl Pts',(-62.31261717248,4.19555285965564,0.623056401494609));
#45538=CARTESIAN_POINT('Ctrl Pts',(-62.19408507323,3.39215244731244,2.5464023350196));
#45539=CARTESIAN_POINT('Ctrl Pts',(-62.0755529739799,1.7695626102988,3.85480365853339));
#45540=CARTESIAN_POINT('Ctrl Pts',(-61.9570208747298,-0.280368567998288,
4.23228738907051));
#45541=CARTESIAN_POINT('Ctrl Pts',(-61.8384887754797,-2.26259200924054,
3.58769291847877));
#45542=CARTESIAN_POINT('Ctrl Pts',(-61.7199566762296,-3.69840974642527,
2.07668688666092));
#45543=CARTESIAN_POINT('Ctrl Pts',(-61.6014245769796,-4.24107831075006,
0.0641703943514818));
#45544=CARTESIAN_POINT('Ctrl Pts',(-61.4828924777294,-3.75954570633811,
-1.96384295703131));
#45545=CARTESIAN_POINT('Ctrl Pts',(-61.3643603784794,-2.3700998720048,-3.51759714491556));
#45546=CARTESIAN_POINT('Ctrl Pts',(-61.2458282792293,-0.408285672900589,
-4.22186758284269));
#45547=CARTESIAN_POINT('Ctrl Pts',(-61.1272961799792,1.65212766441617,-3.90657615556305));
#45548=CARTESIAN_POINT('Ctrl Pts',(-61.0087640807291,3.31355966555602,-2.64786431219091));
#45549=CARTESIAN_POINT('Ctrl Pts',(-60.8902319814791,4.1747820452098,-0.749705251673546));
#45550=CARTESIAN_POINT('Ctrl Pts',(-60.7716998822289,4.02781349732346,1.32950422542484));
#45551=CARTESIAN_POINT('Ctrl Pts',(-60.6531677829789,2.90814627754596,3.08764446455717));
#45552=CARTESIAN_POINT('Ctrl Pts',(-60.5346356837287,1.08617490252564,4.10013257507453));
#45553=CARTESIAN_POINT('Ctrl Pts',(-60.4161035844787,-0.998102733832139,
4.12245727265436));
#45554=CARTESIAN_POINT('Ctrl Pts',(-60.2975714852285,-2.84134318794365,
3.14922724339409));
#45555=CARTESIAN_POINT('Ctrl Pts',(-60.1790393859785,-3.99841195443958,
1.41547312495732));
#45556=CARTESIAN_POINT('Ctrl Pts',(-60.0605072867284,-4.18988277863246,
-0.660111332655873));
#45557=CARTESIAN_POINT('Ctrl Pts',(-59.9419751874784,-3.36951511201551,
-2.57628189458803));
#45558=CARTESIAN_POINT('Ctrl Pts',(-59.8234430882282,-1.73542646721431,
-3.87029207649262));
#45559=CARTESIAN_POINT('Ctrl Pts',(-59.7049109889782,0.317763083477844,
-4.22964426655577));
#45560=CARTESIAN_POINT('Ctrl Pts',(-59.586378889728,2.29420766877876,-3.56755659021834));
#45561=CARTESIAN_POINT('Ctrl Pts',(-59.4678467904781,3.71662484933523,-2.04392011884845));
#45562=CARTESIAN_POINT('Ctrl Pts',(-59.3493146912278,4.24146713027876,-0.0266863449824727));
#45563=CARTESIAN_POINT('Ctrl Pts',(-59.2307825919778,3.74206844848274,1.99699232488131));
#45564=CARTESIAN_POINT('Ctrl Pts',(-59.1122504927277,2.33886818860421,3.53840589673139));
#45565=CARTESIAN_POINT('Ctrl Pts',(-58.9937183934776,0.371062410636318,
4.22531118531867));
#45566=CARTESIAN_POINT('Ctrl Pts',(-58.8751862942276,-1.68680810405213,
3.89182459761031));
#45567=CARTESIAN_POINT('Ctrl Pts',(-58.7961648947275,-2.78637036087181,
3.04285225474445));
#45568=CARTESIAN_POINT('Ctrl Pts',(-58.7566541949775,-3.20225585017534,
2.51287240424535));
#45569=CARTESIAN_POINT('Origin',(0.5,7.95374963839832,-1.25014666726696));
#45570=CARTESIAN_POINT('',(9.,7.8971245663519,-1.27883680879202));
#45571=CARTESIAN_POINT('',(0.499999999999999,7.8971245663519,-1.27883680879202));
#45572=CARTESIAN_POINT('',(4.75,7.8971245663519,-1.27883680879202));
#45573=CARTESIAN_POINT('',(9.,7.73074086114583,-1.3631381946854));
#45574=CARTESIAN_POINT('',(9.,7.95374963839832,-1.25014666726696));
#45575=CARTESIAN_POINT('',(0.5,7.73074086114583,-1.3631381946854));
#45576=CARTESIAN_POINT('',(0.5,7.73074086114583,-1.3631381946854));
#45577=CARTESIAN_POINT('',(0.5,7.95374963839832,-1.25014666726696));
#45578=CARTESIAN_POINT('Origin',(0.5,7.82922163644705,-1.3805030124521));
#45579=CARTESIAN_POINT('',(0.499999999999999,7.85825762906118,-1.49926216363308));
#45580=CARTESIAN_POINT('Origin',(0.5,0.,0.));
#45581=CARTESIAN_POINT('',(0.5,7.73074086114583,-1.3631381946854));
#45582=CARTESIAN_POINT('Origin',(0.5,7.73074086114583,-1.3631381946854));
#45583=CARTESIAN_POINT('',(9.,7.85825762906118,-1.49926216363308));
#45584=CARTESIAN_POINT('',(4.75,7.85825762906118,-1.49926216363308));
#45585=CARTESIAN_POINT('',(9.,7.73074086114583,-1.3631381946854));
#45586=CARTESIAN_POINT('Origin',(9.,7.82922163644705,-1.3805030124521));
#45587=CARTESIAN_POINT('Origin',(9.,0.,0.));
#45588=CARTESIAN_POINT('Origin',(0.5,7.61582861882541,-2.61230826065375));
#45589=CARTESIAN_POINT('',(9.,7.55508181806639,-2.63072969389153));
#45590=CARTESIAN_POINT('',(0.499999999999999,7.55508181806639,-2.63072969389153));
#45591=CARTESIAN_POINT('',(4.75,7.55508181806639,-2.63072969389153));
#45592=CARTESIAN_POINT('',(9.,7.37658707316938,-2.6848581251065));
#45593=CARTESIAN_POINT('',(9.,7.61582861882541,-2.61230826065375));
#45594=CARTESIAN_POINT('',(0.5,7.37658707316938,-2.6848581251065));
#45595=CARTESIAN_POINT('',(0.5,7.37658707316938,-2.6848581251065));
#45596=CARTESIAN_POINT('',(0.5,7.61582861882541,-2.61230826065375));
#45597=CARTESIAN_POINT('Origin',(0.5,7.47055633524797,-2.71906013943907));
#45598=CARTESIAN_POINT('',(0.499999999999999,7.47852889570692,-2.84105711946744));
#45599=CARTESIAN_POINT('Origin',(0.5,0.,0.));
#45600=CARTESIAN_POINT('',(0.5,7.37658707316938,-2.6848581251065));
#45601=CARTESIAN_POINT('Origin',(0.5,7.37658707316938,-2.6848581251065));
#45602=CARTESIAN_POINT('',(9.,7.47852889570692,-2.84105711946744));
#45603=CARTESIAN_POINT('',(4.75,7.47852889570692,-2.84105711946744));
#45604=CARTESIAN_POINT('',(9.,7.37658707316938,-2.6848581251065));
#45605=CARTESIAN_POINT('Origin',(9.,7.47055633524797,-2.71906013943907));
#45606=CARTESIAN_POINT('Origin',(9.,0.,0.));
#45607=CARTESIAN_POINT('Origin',(0.5,7.04650450046473,-3.89509618943234));
#45608=CARTESIAN_POINT('',(9.,6.98348173179481,-3.9026891884556));
#45609=CARTESIAN_POINT('',(0.499999999999999,6.98348173179481,-3.9026891884556));
#45610=CARTESIAN_POINT('',(4.75,6.98348173179481,-3.9026891884556));
#45611=CARTESIAN_POINT('',(9.,6.79829941970784,-3.925));
#45612=CARTESIAN_POINT('',(9.,7.04650450046473,-3.89509618943234));
#45613=CARTESIAN_POINT('',(0.5,6.79829941970784,-3.925));
#45614=CARTESIAN_POINT('',(0.5,6.79829941970784,-3.925));
#45615=CARTESIAN_POINT('',(0.5,7.04650450046473,-3.89509618943234));
#45616=CARTESIAN_POINT('Origin',(0.5,6.88490196008629,-3.975));
#45617=CARTESIAN_POINT('',(0.499999999999999,6.87156884617482,-4.09652799237106));
#45618=CARTESIAN_POINT('Origin',(0.5,0.,0.));
#45619=CARTESIAN_POINT('',(0.5,6.79829941970784,-3.925));
#45620=CARTESIAN_POINT('Origin',(0.5,6.79829941970784,-3.925));
#45621=CARTESIAN_POINT('',(9.,6.87156884617482,-4.09652799237106));
#45622=CARTESIAN_POINT('',(4.75,6.87156884617482,-4.09652799237106));
#45623=CARTESIAN_POINT('',(9.,6.79829941970784,-3.925));
#45624=CARTESIAN_POINT('Origin',(9.,6.88490196008629,-3.975));
#45625=CARTESIAN_POINT('Origin',(9.,0.,0.));
#45626=CARTESIAN_POINT('Origin',(0.5,6.26307590856075,-5.0595335915088));
#45627=CARTESIAN_POINT('',(9.,6.1996920869149,-5.05606744688446));
#45628=CARTESIAN_POINT('',(0.499999999999999,6.1996920869149,-5.05606744688446));
#45629=CARTESIAN_POINT('',(4.75,6.1996920869149,-5.05606744688446));
#45630=CARTESIAN_POINT('',(9.,6.01344887848397,-5.04588273603934));
#45631=CARTESIAN_POINT('',(9.,6.26307590856075,-5.0595335915088));
#45632=CARTESIAN_POINT('',(0.5,6.01344887848397,-5.04588273603934));
#45633=CARTESIAN_POINT('',(0.5,6.01344887848397,-5.04588273603934));
#45634=CARTESIAN_POINT('',(0.5,6.26307590856075,-5.0595335915088));
#45635=CARTESIAN_POINT('Origin',(0.5,6.09005332279587,-5.11016149700799));
#45636=CARTESIAN_POINT('',(0.499999999999999,6.05581965443331,-5.22752793516966));
#45637=CARTESIAN_POINT('Origin',(0.5,0.,0.));
#45638=CARTESIAN_POINT('',(0.5,6.01344887848397,-5.04588273603934));
#45639=CARTESIAN_POINT('Origin',(0.5,6.01344887848397,-5.04588273603934));
#45640=CARTESIAN_POINT('',(9.,6.05581965443331,-5.22752793516966));
#45641=CARTESIAN_POINT('',(4.75,6.05581965443331,-5.22752793516966));
#45642=CARTESIAN_POINT('',(9.,6.01344887848397,-5.04588273603934));
#45643=CARTESIAN_POINT('Origin',(9.,6.09005332279587,-5.11016149700799));
#45644=CARTESIAN_POINT('Origin',(9.,0.,0.));
#45645=CARTESIAN_POINT('Origin',(0.5,5.28934692444449,-6.07023962565479));
#45646=CARTESIAN_POINT('',(9.,5.22752793516966,-6.05581965443332));
#45647=CARTESIAN_POINT('',(0.499999999999999,5.22752793516966,-6.05581965443332));
#45648=CARTESIAN_POINT('',(4.75,5.22752793516966,-6.05581965443332));
#45649=CARTESIAN_POINT('',(9.,5.04588273603933,-6.01344887848398));
#45650=CARTESIAN_POINT('',(9.,5.28934692444449,-6.07023962565479));
#45651=CARTESIAN_POINT('',(0.5,5.04588273603933,-6.01344887848398));
#45652=CARTESIAN_POINT('',(0.5,5.04588273603933,-6.01344887848398));
#45653=CARTESIAN_POINT('',(0.5,5.28934692444449,-6.07023962565479));
#45654=CARTESIAN_POINT('Origin',(0.5,5.11016149700799,-6.09005332279588));
#45655=CARTESIAN_POINT('',(0.499999999999999,5.05606744688446,-6.19969208691491));
#45656=CARTESIAN_POINT('Origin',(0.5,0.,0.));
#45657=CARTESIAN_POINT('',(0.5,5.04588273603933,-6.01344887848398));
#45658=CARTESIAN_POINT('Origin',(0.5,5.04588273603933,-6.01344887848398));
#45659=CARTESIAN_POINT('',(9.,5.05606744688446,-6.19969208691491));
#45660=CARTESIAN_POINT('',(4.75,5.05606744688446,-6.19969208691491));
#45661=CARTESIAN_POINT('',(9.,5.04588273603933,-6.01344887848398));
#45662=CARTESIAN_POINT('Origin',(9.,5.11016149700799,-6.09005332279588));
#45663=CARTESIAN_POINT('Origin',(9.,0.,0.));
#45664=CARTESIAN_POINT('Origin',(0.5,4.15490381056767,-6.89650450046473));
#45665=CARTESIAN_POINT('',(9.,4.09652799237105,-6.87156884617482));
#45666=CARTESIAN_POINT('',(0.499999999999999,4.09652799237105,-6.87156884617482));
#45667=CARTESIAN_POINT('',(4.75,4.09652799237105,-6.87156884617482));
#45668=CARTESIAN_POINT('',(9.,3.925,-6.79829941970784));
#45669=CARTESIAN_POINT('',(9.,4.15490381056767,-6.89650450046473));
#45670=CARTESIAN_POINT('',(0.5,3.925,-6.79829941970784));
#45671=CARTESIAN_POINT('',(0.5,3.925,-6.79829941970784));
#45672=CARTESIAN_POINT('',(0.5,4.15490381056767,-6.89650450046473));
#45673=CARTESIAN_POINT('Origin',(0.5,3.975,-6.88490196008629));
#45674=CARTESIAN_POINT('',(0.499999999999999,3.9026891884556,-6.98348173179481));
#45675=CARTESIAN_POINT('Origin',(0.5,0.,0.));
#45676=CARTESIAN_POINT('',(0.5,3.925,-6.79829941970784));
#45677=CARTESIAN_POINT('Origin',(0.5,3.925,-6.79829941970784));
#45678=CARTESIAN_POINT('',(9.,3.9026891884556,-6.98348173179481));
#45679=CARTESIAN_POINT('',(4.75,3.9026891884556,-6.98348173179481));
#45680=CARTESIAN_POINT('',(9.,3.925,-6.79829941970784));
#45681=CARTESIAN_POINT('Origin',(9.,3.975,-6.88490196008629));
#45682=CARTESIAN_POINT('Origin',(9.,0.,0.));
#45683=CARTESIAN_POINT('Origin',(0.5,2.89421604688952,-7.51322257582772));
#45684=CARTESIAN_POINT('',(9.,2.84105711946744,-7.47852889570692));
#45685=CARTESIAN_POINT('',(0.499999999999999,2.84105711946744,-7.47852889570692));
#45686=CARTESIAN_POINT('',(4.75,2.84105711946744,-7.47852889570692));
#45687=CARTESIAN_POINT('',(9.,2.6848581251065,-7.37658707316938));
#45688=CARTESIAN_POINT('',(9.,2.89421604688952,-7.51322257582772));
#45689=CARTESIAN_POINT('',(0.5,2.6848581251065,-7.37658707316938));
#45690=CARTESIAN_POINT('',(0.5,2.6848581251065,-7.37658707316938));
#45691=CARTESIAN_POINT('',(0.5,2.89421604688952,-7.51322257582772));
#45692=CARTESIAN_POINT('Origin',(0.5,2.71906013943906,-7.47055633524797));
#45693=CARTESIAN_POINT('',(0.499999999999999,2.63072969389152,-7.5550818180664));
#45694=CARTESIAN_POINT('Origin',(0.5,0.,0.));
#45695=CARTESIAN_POINT('',(0.5,2.6848581251065,-7.37658707316938));
#45696=CARTESIAN_POINT('Origin',(0.5,2.6848581251065,-7.37658707316938));
#45697=CARTESIAN_POINT('',(9.,2.63072969389152,-7.5550818180664));
#45698=CARTESIAN_POINT('',(4.75,2.63072969389152,-7.5550818180664));
#45699=CARTESIAN_POINT('',(9.,2.6848581251065,-7.37658707316938));
#45700=CARTESIAN_POINT('Origin',(9.,2.71906013943906,-7.47055633524797));
#45701=CARTESIAN_POINT('Origin',(9.,0.,0.));
#45702=CARTESIAN_POINT('Origin',(0.5,1.54558899317062,-7.90165518509824));
#45703=CARTESIAN_POINT('',(9.,1.49926216363307,-7.85825762906118));
#45704=CARTESIAN_POINT('',(0.499999999999999,1.49926216363307,-7.85825762906118));
#45705=CARTESIAN_POINT('',(4.75,1.49926216363307,-7.85825762906118));
#45706=CARTESIAN_POINT('',(9.,1.3631381946854,-7.73074086114583));
#45707=CARTESIAN_POINT('',(9.,1.54558899317062,-7.90165518509824));
#45708=CARTESIAN_POINT('',(0.5,1.3631381946854,-7.73074086114583));
#45709=CARTESIAN_POINT('',(0.5,1.3631381946854,-7.73074086114583));
#45710=CARTESIAN_POINT('',(0.5,1.54558899317062,-7.90165518509824));
#45711=CARTESIAN_POINT('Origin',(0.5,1.38050301245209,-7.82922163644705));
#45712=CARTESIAN_POINT('',(0.499999999999999,1.27883680879201,-7.8971245663519));
#45713=CARTESIAN_POINT('Origin',(0.5,0.,0.));
#45714=CARTESIAN_POINT('',(0.5,1.3631381946854,-7.73074086114583));
#45715=CARTESIAN_POINT('Origin',(0.5,1.3631381946854,-7.73074086114583));
#45716=CARTESIAN_POINT('',(9.,1.27883680879201,-7.8971245663519));
#45717=CARTESIAN_POINT('',(4.75,1.27883680879201,-7.8971245663519));
#45718=CARTESIAN_POINT('',(9.,1.3631381946854,-7.73074086114583));
#45719=CARTESIAN_POINT('Origin',(9.,1.38050301245209,-7.82922163644705));
#45720=CARTESIAN_POINT('Origin',(9.,0.,0.));
#45721=CARTESIAN_POINT('Origin',(0.5,0.149999999999999,-8.05));
#45722=CARTESIAN_POINT('',(9.,0.111912885619984,-7.99921718082665));
#45723=CARTESIAN_POINT('',(0.499999999999999,0.111912885619984,-7.99921718082665));
#45724=CARTESIAN_POINT('',(4.75,0.111912885619984,-7.99921718082665));
#45725=CARTESIAN_POINT('',(9.,-1.44202160599601E-15,-7.85));
#45726=CARTESIAN_POINT('',(9.,0.149999999999999,-8.05));
#45727=CARTESIAN_POINT('',(0.5,-1.44202160599601E-15,-7.85));
#45728=CARTESIAN_POINT('',(0.5,-1.44202160599601E-15,-7.85));
#45729=CARTESIAN_POINT('',(0.5,0.149999999999999,-8.05));
#45730=CARTESIAN_POINT('Origin',(0.5,-1.46039130798322E-15,-7.95));
#45731=CARTESIAN_POINT('',(0.499999999999999,-0.111912885619986,-7.99921718082665));
#45732=CARTESIAN_POINT('Origin',(0.5,0.,0.));
#45733=CARTESIAN_POINT('',(0.5,-1.44202160599601E-15,-7.85));
#45734=CARTESIAN_POINT('Origin',(0.5,-1.44202160599601E-15,-7.85));
#45735=CARTESIAN_POINT('',(9.,-0.111912885619986,-7.99921718082665));
#45736=CARTESIAN_POINT('',(4.75,-0.111912885619986,-7.99921718082665));
#45737=CARTESIAN_POINT('',(9.,-1.44202160599601E-15,-7.85));
#45738=CARTESIAN_POINT('Origin',(9.,-1.46039130798322E-15,-7.95));
#45739=CARTESIAN_POINT('Origin',(9.,0.,0.));
#45740=CARTESIAN_POINT('Origin',(0.5,-1.25014666726696,-7.95374963839832));
#45741=CARTESIAN_POINT('',(9.,-1.27883680879202,-7.8971245663519));
#45742=CARTESIAN_POINT('',(0.499999999999999,-1.27883680879202,-7.8971245663519));
#45743=CARTESIAN_POINT('',(4.75,-1.27883680879202,-7.8971245663519));
#45744=CARTESIAN_POINT('',(9.,-1.3631381946854,-7.73074086114583));
#45745=CARTESIAN_POINT('',(9.,-1.25014666726696,-7.95374963839832));
#45746=CARTESIAN_POINT('',(0.5,-1.3631381946854,-7.73074086114583));
#45747=CARTESIAN_POINT('',(0.5,-1.3631381946854,-7.73074086114583));
#45748=CARTESIAN_POINT('',(0.5,-1.25014666726696,-7.95374963839832));
#45749=CARTESIAN_POINT('Origin',(0.5,-1.3805030124521,-7.82922163644705));
#45750=CARTESIAN_POINT('',(0.499999999999999,-1.49926216363308,-7.85825762906118));
#45751=CARTESIAN_POINT('Origin',(0.5,0.,0.));
#45752=CARTESIAN_POINT('',(0.5,-1.3631381946854,-7.73074086114583));
#45753=CARTESIAN_POINT('Origin',(0.5,-1.3631381946854,-7.73074086114583));
#45754=CARTESIAN_POINT('',(9.,-1.49926216363308,-7.85825762906118));
#45755=CARTESIAN_POINT('',(4.75,-1.49926216363308,-7.85825762906118));
#45756=CARTESIAN_POINT('',(9.,-1.3631381946854,-7.73074086114583));
#45757=CARTESIAN_POINT('Origin',(9.,-1.3805030124521,-7.82922163644705));
#45758=CARTESIAN_POINT('Origin',(9.,0.,0.));
#45759=CARTESIAN_POINT('Origin',(0.5,-2.61230826065375,-7.61582861882541));
#45760=CARTESIAN_POINT('',(9.,-2.63072969389153,-7.55508181806639));
#45761=CARTESIAN_POINT('',(0.499999999999999,-2.63072969389153,-7.55508181806639));
#45762=CARTESIAN_POINT('',(4.75,-2.63072969389153,-7.55508181806639));
#45763=CARTESIAN_POINT('',(9.,-2.6848581251065,-7.37658707316938));
#45764=CARTESIAN_POINT('',(9.,-2.61230826065375,-7.61582861882541));
#45765=CARTESIAN_POINT('',(0.5,-2.6848581251065,-7.37658707316938));
#45766=CARTESIAN_POINT('',(0.5,-2.6848581251065,-7.37658707316938));
#45767=CARTESIAN_POINT('',(0.5,-2.61230826065375,-7.61582861882541));
#45768=CARTESIAN_POINT('Origin',(0.5,-2.71906013943907,-7.47055633524797));
#45769=CARTESIAN_POINT('',(0.499999999999999,-2.84105711946745,-7.47852889570692));
#45770=CARTESIAN_POINT('Origin',(0.5,0.,0.));
#45771=CARTESIAN_POINT('',(0.5,-2.6848581251065,-7.37658707316938));
#45772=CARTESIAN_POINT('Origin',(0.5,-2.6848581251065,-7.37658707316938));
#45773=CARTESIAN_POINT('',(9.,-2.84105711946745,-7.47852889570692));
#45774=CARTESIAN_POINT('',(4.75,-2.84105711946744,-7.47852889570692));
#45775=CARTESIAN_POINT('',(9.,-2.6848581251065,-7.37658707316938));
#45776=CARTESIAN_POINT('Origin',(9.,-2.71906013943907,-7.47055633524797));
#45777=CARTESIAN_POINT('Origin',(9.,0.,0.));
#45778=CARTESIAN_POINT('Origin',(0.5,-3.89509618943234,-7.04650450046473));
#45779=CARTESIAN_POINT('',(9.,-3.9026891884556,-6.98348173179481));
#45780=CARTESIAN_POINT('',(0.499999999999999,-3.9026891884556,-6.98348173179481));
#45781=CARTESIAN_POINT('',(4.75,-3.9026891884556,-6.98348173179481));
#45782=CARTESIAN_POINT('',(9.,-3.925,-6.79829941970784));
#45783=CARTESIAN_POINT('',(9.,-3.89509618943234,-7.04650450046473));
#45784=CARTESIAN_POINT('',(0.5,-3.925,-6.79829941970784));
#45785=CARTESIAN_POINT('',(0.5,-3.925,-6.79829941970784));
#45786=CARTESIAN_POINT('',(0.5,-3.89509618943234,-7.04650450046473));
#45787=CARTESIAN_POINT('Origin',(0.5,-3.975,-6.88490196008629));
#45788=CARTESIAN_POINT('',(0.499999999999999,-4.09652799237106,-6.87156884617482));
#45789=CARTESIAN_POINT('Origin',(0.5,0.,0.));
#45790=CARTESIAN_POINT('',(0.5,-3.925,-6.79829941970784));
#45791=CARTESIAN_POINT('Origin',(0.5,-3.925,-6.79829941970784));
#45792=CARTESIAN_POINT('',(9.,-4.09652799237106,-6.87156884617482));
#45793=CARTESIAN_POINT('',(4.75,-4.09652799237106,-6.87156884617482));
#45794=CARTESIAN_POINT('',(9.,-3.925,-6.79829941970784));
#45795=CARTESIAN_POINT('Origin',(9.,-3.975,-6.88490196008629));
#45796=CARTESIAN_POINT('Origin',(9.,0.,0.));
#45797=CARTESIAN_POINT('Origin',(0.5,-5.0595335915088,-6.26307590856075));
#45798=CARTESIAN_POINT('',(9.,-5.05606744688446,-6.1996920869149));
#45799=CARTESIAN_POINT('',(0.499999999999999,-5.05606744688446,-6.1996920869149));
#45800=CARTESIAN_POINT('',(4.75,-5.05606744688446,-6.1996920869149));
#45801=CARTESIAN_POINT('',(9.,-5.04588273603933,-6.01344887848398));
#45802=CARTESIAN_POINT('',(9.,-5.0595335915088,-6.26307590856075));
#45803=CARTESIAN_POINT('',(0.5,-5.04588273603933,-6.01344887848398));
#45804=CARTESIAN_POINT('',(0.5,-5.04588273603933,-6.01344887848398));
#45805=CARTESIAN_POINT('',(0.5,-5.0595335915088,-6.26307590856075));
#45806=CARTESIAN_POINT('Origin',(0.5,-5.11016149700799,-6.09005332279587));
#45807=CARTESIAN_POINT('',(0.499999999999999,-5.22752793516966,-6.05581965443332));
#45808=CARTESIAN_POINT('Origin',(0.5,0.,0.));
#45809=CARTESIAN_POINT('',(0.5,-5.04588273603933,-6.01344887848398));
#45810=CARTESIAN_POINT('Origin',(0.5,-5.04588273603933,-6.01344887848398));
#45811=CARTESIAN_POINT('',(9.,-5.22752793516966,-6.05581965443332));
#45812=CARTESIAN_POINT('',(4.75,-5.22752793516966,-6.05581965443332));
#45813=CARTESIAN_POINT('',(9.,-5.04588273603933,-6.01344887848398));
#45814=CARTESIAN_POINT('Origin',(9.,-5.11016149700799,-6.09005332279587));
#45815=CARTESIAN_POINT('Origin',(9.,0.,0.));
#45816=CARTESIAN_POINT('Origin',(0.5,-6.07023962565479,-5.28934692444449));
#45817=CARTESIAN_POINT('',(9.,-6.05581965443332,-5.22752793516966));
#45818=CARTESIAN_POINT('',(0.499999999999999,-6.05581965443332,-5.22752793516966));
#45819=CARTESIAN_POINT('',(4.75,-6.05581965443332,-5.22752793516966));
#45820=CARTESIAN_POINT('',(9.,-6.01344887848398,-5.04588273603933));
#45821=CARTESIAN_POINT('',(9.,-6.07023962565479,-5.28934692444449));
#45822=CARTESIAN_POINT('',(0.5,-6.01344887848398,-5.04588273603933));
#45823=CARTESIAN_POINT('',(0.5,-6.01344887848398,-5.04588273603933));
#45824=CARTESIAN_POINT('',(0.5,-6.07023962565479,-5.28934692444449));
#45825=CARTESIAN_POINT('Origin',(0.5,-6.09005332279588,-5.11016149700799));
#45826=CARTESIAN_POINT('',(0.499999999999999,-6.1996920869149,-5.05606744688446));
#45827=CARTESIAN_POINT('Origin',(0.5,0.,0.));
#45828=CARTESIAN_POINT('',(0.5,-6.01344887848398,-5.04588273603933));
#45829=CARTESIAN_POINT('Origin',(0.5,-6.01344887848398,-5.04588273603933));
#45830=CARTESIAN_POINT('',(9.,-6.1996920869149,-5.05606744688446));
#45831=CARTESIAN_POINT('',(4.75,-6.1996920869149,-5.05606744688446));
#45832=CARTESIAN_POINT('',(9.,-6.01344887848398,-5.04588273603933));
#45833=CARTESIAN_POINT('Origin',(9.,-6.09005332279588,-5.11016149700799));
#45834=CARTESIAN_POINT('Origin',(9.,0.,0.));
#45835=CARTESIAN_POINT('Origin',(0.5,-6.89650450046473,-4.15490381056766));
#45836=CARTESIAN_POINT('',(9.,-6.87156884617482,-4.09652799237105));
#45837=CARTESIAN_POINT('',(0.499999999999999,-6.87156884617482,-4.09652799237105));
#45838=CARTESIAN_POINT('',(4.75,-6.87156884617482,-4.09652799237105));
#45839=CARTESIAN_POINT('',(9.,-6.79829941970784,-3.925));
#45840=CARTESIAN_POINT('',(9.,-6.89650450046473,-4.15490381056766));
#45841=CARTESIAN_POINT('',(0.5,-6.79829941970784,-3.925));
#45842=CARTESIAN_POINT('',(0.5,-6.79829941970784,-3.925));
#45843=CARTESIAN_POINT('',(0.5,-6.89650450046473,-4.15490381056766));
#45844=CARTESIAN_POINT('Origin',(0.5,-6.88490196008629,-3.975));
#45845=CARTESIAN_POINT('',(0.499999999999999,-6.98348173179481,-3.90268918845559));
#45846=CARTESIAN_POINT('Origin',(0.5,0.,0.));
#45847=CARTESIAN_POINT('',(0.5,-6.79829941970784,-3.925));
#45848=CARTESIAN_POINT('Origin',(0.5,-6.79829941970784,-3.925));
#45849=CARTESIAN_POINT('',(9.,-6.98348173179481,-3.90268918845559));
#45850=CARTESIAN_POINT('',(4.75,-6.98348173179481,-3.90268918845559));
#45851=CARTESIAN_POINT('',(9.,-6.79829941970784,-3.925));
#45852=CARTESIAN_POINT('Origin',(9.,-6.88490196008629,-3.975));
#45853=CARTESIAN_POINT('Origin',(9.,0.,0.));
#45854=CARTESIAN_POINT('Origin',(0.5,-7.51322257582771,-2.89421604688952));
#45855=CARTESIAN_POINT('',(9.,-7.47852889570692,-2.84105711946744));
#45856=CARTESIAN_POINT('',(0.499999999999999,-7.47852889570692,-2.84105711946744));
#45857=CARTESIAN_POINT('',(4.75,-7.47852889570692,-2.84105711946744));
#45858=CARTESIAN_POINT('',(9.,-7.37658707316938,-2.6848581251065));
#45859=CARTESIAN_POINT('',(9.,-7.51322257582771,-2.89421604688952));
#45860=CARTESIAN_POINT('',(0.5,-7.37658707316938,-2.6848581251065));
#45861=CARTESIAN_POINT('',(0.5,-7.37658707316938,-2.6848581251065));
#45862=CARTESIAN_POINT('',(0.5,-7.51322257582771,-2.89421604688952));
#45863=CARTESIAN_POINT('Origin',(0.5,-7.47055633524797,-2.71906013943907));
#45864=CARTESIAN_POINT('',(0.499999999999999,-7.55508181806639,-2.63072969389152));
#45865=CARTESIAN_POINT('Origin',(0.5,0.,0.));
#45866=CARTESIAN_POINT('',(0.5,-7.37658707316938,-2.6848581251065));
#45867=CARTESIAN_POINT('Origin',(0.5,-7.37658707316938,-2.6848581251065));
#45868=CARTESIAN_POINT('',(9.,-7.55508181806639,-2.63072969389152));
#45869=CARTESIAN_POINT('',(4.75,-7.55508181806639,-2.63072969389152));
#45870=CARTESIAN_POINT('',(9.,-7.37658707316938,-2.6848581251065));
#45871=CARTESIAN_POINT('Origin',(9.,-7.47055633524797,-2.71906013943907));
#45872=CARTESIAN_POINT('Origin',(9.,0.,0.));
#45873=CARTESIAN_POINT('Origin',(0.5,-7.90165518509824,-1.54558899317062));
#45874=CARTESIAN_POINT('',(9.,-7.85825762906118,-1.49926216363307));
#45875=CARTESIAN_POINT('',(0.499999999999999,-7.85825762906118,-1.49926216363307));
#45876=CARTESIAN_POINT('',(4.75,-7.85825762906118,-1.49926216363307));
#45877=CARTESIAN_POINT('',(9.,-7.73074086114583,-1.3631381946854));
#45878=CARTESIAN_POINT('',(9.,-7.90165518509824,-1.54558899317062));
#45879=CARTESIAN_POINT('',(0.5,-7.73074086114583,-1.3631381946854));
#45880=CARTESIAN_POINT('',(0.5,-7.73074086114583,-1.3631381946854));
#45881=CARTESIAN_POINT('',(0.5,-7.90165518509824,-1.54558899317062));
#45882=CARTESIAN_POINT('Origin',(0.5,-7.82922163644705,-1.38050301245209));
#45883=CARTESIAN_POINT('',(0.499999999999999,-7.8971245663519,-1.27883680879201));
#45884=CARTESIAN_POINT('Origin',(0.5,0.,0.));
#45885=CARTESIAN_POINT('',(0.5,-7.73074086114583,-1.3631381946854));
#45886=CARTESIAN_POINT('Origin',(0.5,-7.73074086114583,-1.3631381946854));
#45887=CARTESIAN_POINT('',(9.,-7.8971245663519,-1.27883680879201));
#45888=CARTESIAN_POINT('',(4.75,-7.8971245663519,-1.27883680879201));
#45889=CARTESIAN_POINT('',(9.,-7.73074086114583,-1.3631381946854));
#45890=CARTESIAN_POINT('Origin',(9.,-7.82922163644705,-1.38050301245209));
#45891=CARTESIAN_POINT('Origin',(9.,0.,0.));
#45892=CARTESIAN_POINT('Origin',(0.5,-8.05,-0.149999999999999));
#45893=CARTESIAN_POINT('',(9.,-7.99921718082665,-0.111912885619986));
#45894=CARTESIAN_POINT('',(0.499999999999999,-7.99921718082665,-0.111912885619986));
#45895=CARTESIAN_POINT('',(4.75,-7.99921718082665,-0.111912885619986));
#45896=CARTESIAN_POINT('',(9.,-7.85,9.61347737330672E-16));
#45897=CARTESIAN_POINT('',(9.,-8.05,-0.149999999999999));
#45898=CARTESIAN_POINT('',(0.5,-7.85,9.61347737330672E-16));
#45899=CARTESIAN_POINT('',(0.5,-7.85,9.61347737330672E-16));
#45900=CARTESIAN_POINT('',(0.5,-8.05,-0.149999999999999));
#45901=CARTESIAN_POINT('Origin',(0.5,-7.95,9.73594205322146E-16));
#45902=CARTESIAN_POINT('',(0.5,-8.,-9.79717439317883E-16));
#45903=CARTESIAN_POINT('Origin',(0.5,0.,0.));
#45904=CARTESIAN_POINT('',(0.499999999999999,-7.99921718082665,0.111912885619986));
#45905=CARTESIAN_POINT('',(0.5,-7.85,9.61347737330672E-16));
#45906=CARTESIAN_POINT('Origin',(0.5,0.,0.));
#45907=CARTESIAN_POINT('Origin',(0.5,-7.85,9.61347737330672E-16));
#45908=CARTESIAN_POINT('',(9.,-7.99921718082665,0.111912885619986));
#45909=CARTESIAN_POINT('',(4.75,-7.99921718082665,0.111912885619986));
#45910=CARTESIAN_POINT('',(9.,-7.85,9.61347737330672E-16));
#45911=CARTESIAN_POINT('Origin',(9.,-7.95,9.73594205322146E-16));
#45912=CARTESIAN_POINT('',(9.,-8.,-9.79717439317883E-16));
#45913=CARTESIAN_POINT('Origin',(9.,0.,0.));
#45914=CARTESIAN_POINT('Origin',(9.,0.,0.));
#45915=CARTESIAN_POINT('Origin',(0.5,-7.95374963839832,1.25014666726696));
#45916=CARTESIAN_POINT('',(9.,-7.8971245663519,1.27883680879202));
#45917=CARTESIAN_POINT('',(0.499999999999999,-7.8971245663519,1.27883680879202));
#45918=CARTESIAN_POINT('',(4.75,-7.8971245663519,1.27883680879202));
#45919=CARTESIAN_POINT('',(9.,-7.73074086114583,1.36313819468541));
#45920=CARTESIAN_POINT('',(9.,-7.95374963839832,1.25014666726696));
#45921=CARTESIAN_POINT('',(0.5,-7.73074086114583,1.36313819468541));
#45922=CARTESIAN_POINT('',(0.5,-7.73074086114583,1.36313819468541));
#45923=CARTESIAN_POINT('',(0.5,-7.95374963839832,1.25014666726696));
#45924=CARTESIAN_POINT('Origin',(0.5,-7.82922163644705,1.3805030124521));
#45925=CARTESIAN_POINT('',(0.499999999999999,-7.85825762906118,1.49926216363308));
#45926=CARTESIAN_POINT('Origin',(0.5,0.,0.));
#45927=CARTESIAN_POINT('',(0.5,-7.73074086114583,1.36313819468541));
#45928=CARTESIAN_POINT('Origin',(0.5,-7.73074086114583,1.36313819468541));
#45929=CARTESIAN_POINT('',(9.,-7.85825762906118,1.49926216363308));
#45930=CARTESIAN_POINT('',(4.75,-7.85825762906118,1.49926216363308));
#45931=CARTESIAN_POINT('',(9.,-7.73074086114583,1.36313819468541));
#45932=CARTESIAN_POINT('Origin',(9.,-7.82922163644705,1.3805030124521));
#45933=CARTESIAN_POINT('Origin',(9.,0.,0.));
#45934=CARTESIAN_POINT('Origin',(0.5,-7.61582861882541,2.61230826065375));
#45935=CARTESIAN_POINT('',(9.,-7.55508181806639,2.63072969389153));
#45936=CARTESIAN_POINT('',(0.499999999999999,-7.55508181806639,2.63072969389153));
#45937=CARTESIAN_POINT('',(4.75,-7.55508181806639,2.63072969389153));
#45938=CARTESIAN_POINT('',(9.,-7.37658707316938,2.6848581251065));
#45939=CARTESIAN_POINT('',(9.,-7.61582861882541,2.61230826065375));
#45940=CARTESIAN_POINT('',(0.5,-7.37658707316938,2.6848581251065));
#45941=CARTESIAN_POINT('',(0.5,-7.37658707316938,2.6848581251065));
#45942=CARTESIAN_POINT('',(0.5,-7.61582861882541,2.61230826065375));
#45943=CARTESIAN_POINT('Origin',(0.5,-7.47055633524797,2.71906013943907));
#45944=CARTESIAN_POINT('',(0.499999999999999,-7.47852889570692,2.84105711946744));
#45945=CARTESIAN_POINT('Origin',(0.5,0.,0.));
#45946=CARTESIAN_POINT('',(0.5,-7.37658707316938,2.6848581251065));
#45947=CARTESIAN_POINT('Origin',(0.5,-7.37658707316938,2.6848581251065));
#45948=CARTESIAN_POINT('',(9.,-7.47852889570692,2.84105711946744));
#45949=CARTESIAN_POINT('',(4.75,-7.47852889570692,2.84105711946744));
#45950=CARTESIAN_POINT('',(9.,-7.37658707316938,2.6848581251065));
#45951=CARTESIAN_POINT('Origin',(9.,-7.47055633524797,2.71906013943907));
#45952=CARTESIAN_POINT('Origin',(9.,0.,0.));
#45953=CARTESIAN_POINT('Origin',(0.5,-7.04650450046473,3.89509618943233));
#45954=CARTESIAN_POINT('',(9.,-6.98348173179481,3.90268918845559));
#45955=CARTESIAN_POINT('',(0.499999999999999,-6.98348173179481,3.90268918845559));
#45956=CARTESIAN_POINT('',(4.75,-6.98348173179481,3.90268918845559));
#45957=CARTESIAN_POINT('',(9.,-6.79829941970784,3.925));
#45958=CARTESIAN_POINT('',(9.,-7.04650450046473,3.89509618943233));
#45959=CARTESIAN_POINT('',(0.5,-6.79829941970784,3.925));
#45960=CARTESIAN_POINT('',(0.5,-6.79829941970784,3.925));
#45961=CARTESIAN_POINT('',(0.5,-7.04650450046473,3.89509618943233));
#45962=CARTESIAN_POINT('Origin',(0.5,-6.88490196008629,3.975));
#45963=CARTESIAN_POINT('',(0.499999999999999,-6.87156884617482,4.09652799237105));
#45964=CARTESIAN_POINT('Origin',(0.5,0.,0.));
#45965=CARTESIAN_POINT('',(0.5,-6.79829941970784,3.925));
#45966=CARTESIAN_POINT('Origin',(0.5,-6.79829941970784,3.925));
#45967=CARTESIAN_POINT('',(9.,-6.87156884617482,4.09652799237105));
#45968=CARTESIAN_POINT('',(4.75,-6.87156884617482,4.09652799237105));
#45969=CARTESIAN_POINT('',(9.,-6.79829941970784,3.925));
#45970=CARTESIAN_POINT('Origin',(9.,-6.88490196008629,3.975));
#45971=CARTESIAN_POINT('Origin',(9.,0.,0.));
#45972=CARTESIAN_POINT('Origin',(0.5,-6.26307590856075,5.0595335915088));
#45973=CARTESIAN_POINT('',(9.,-6.1996920869149,5.05606744688446));
#45974=CARTESIAN_POINT('',(0.499999999999999,-6.1996920869149,5.05606744688446));
#45975=CARTESIAN_POINT('',(4.75,-6.1996920869149,5.05606744688446));
#45976=CARTESIAN_POINT('',(9.,-6.01344887848398,5.04588273603933));
#45977=CARTESIAN_POINT('',(9.,-6.26307590856075,5.0595335915088));
#45978=CARTESIAN_POINT('',(0.5,-6.01344887848398,5.04588273603933));
#45979=CARTESIAN_POINT('',(0.5,-6.01344887848398,5.04588273603933));
#45980=CARTESIAN_POINT('',(0.5,-6.26307590856075,5.0595335915088));
#45981=CARTESIAN_POINT('Origin',(0.5,-6.09005332279587,5.11016149700799));
#45982=CARTESIAN_POINT('',(0.499999999999999,-6.05581965443332,5.22752793516966));
#45983=CARTESIAN_POINT('Origin',(0.5,0.,0.));
#45984=CARTESIAN_POINT('',(0.5,-6.01344887848398,5.04588273603933));
#45985=CARTESIAN_POINT('Origin',(0.5,-6.01344887848398,5.04588273603933));
#45986=CARTESIAN_POINT('',(9.,-6.05581965443332,5.22752793516966));
#45987=CARTESIAN_POINT('',(4.75,-6.05581965443332,5.22752793516966));
#45988=CARTESIAN_POINT('',(9.,-6.01344887848398,5.04588273603933));
#45989=CARTESIAN_POINT('Origin',(9.,-6.09005332279587,5.11016149700799));
#45990=CARTESIAN_POINT('Origin',(9.,0.,0.));
#45991=CARTESIAN_POINT('Origin',(0.5,-5.28934692444449,6.07023962565479));
#45992=CARTESIAN_POINT('',(9.,-5.22752793516966,6.05581965443332));
#45993=CARTESIAN_POINT('',(0.499999999999999,-5.22752793516966,6.05581965443332));
#45994=CARTESIAN_POINT('',(4.75,-5.22752793516966,6.05581965443332));
#45995=CARTESIAN_POINT('',(9.,-5.04588273603933,6.01344887848398));
#45996=CARTESIAN_POINT('',(9.,-5.28934692444449,6.07023962565479));
#45997=CARTESIAN_POINT('',(0.5,-5.04588273603933,6.01344887848398));
#45998=CARTESIAN_POINT('',(0.5,-5.04588273603933,6.01344887848398));
#45999=CARTESIAN_POINT('',(0.5,-5.28934692444449,6.07023962565479));
#46000=CARTESIAN_POINT('Origin',(0.5,-5.11016149700799,6.09005332279587));
#46001=CARTESIAN_POINT('',(0.499999999999999,-5.05606744688446,6.1996920869149));
#46002=CARTESIAN_POINT('Origin',(0.5,0.,0.));
#46003=CARTESIAN_POINT('',(0.5,-5.04588273603933,6.01344887848398));
#46004=CARTESIAN_POINT('Origin',(0.5,-5.04588273603933,6.01344887848398));
#46005=CARTESIAN_POINT('',(9.,-5.05606744688446,6.1996920869149));
#46006=CARTESIAN_POINT('',(4.75,-5.05606744688446,6.1996920869149));
#46007=CARTESIAN_POINT('',(9.,-5.04588273603933,6.01344887848398));
#46008=CARTESIAN_POINT('Origin',(9.,-5.11016149700799,6.09005332279587));
#46009=CARTESIAN_POINT('Origin',(9.,0.,0.));
#46010=CARTESIAN_POINT('Origin',(0.5,-4.15490381056767,6.89650450046473));
#46011=CARTESIAN_POINT('',(9.,-4.09652799237105,6.87156884617482));
#46012=CARTESIAN_POINT('',(0.499999999999999,-4.09652799237105,6.87156884617482));
#46013=CARTESIAN_POINT('',(4.75,-4.09652799237105,6.87156884617482));
#46014=CARTESIAN_POINT('',(9.,-3.925,6.79829941970784));
#46015=CARTESIAN_POINT('',(9.,-4.15490381056767,6.89650450046473));
#46016=CARTESIAN_POINT('',(0.5,-3.925,6.79829941970784));
#46017=CARTESIAN_POINT('',(0.5,-3.925,6.79829941970784));
#46018=CARTESIAN_POINT('',(0.5,-4.15490381056767,6.89650450046473));
#46019=CARTESIAN_POINT('Origin',(0.5,-3.975,6.88490196008629));
#46020=CARTESIAN_POINT('',(0.499999999999999,-3.90268918845559,6.98348173179481));
#46021=CARTESIAN_POINT('Origin',(0.5,0.,0.));
#46022=CARTESIAN_POINT('',(0.5,-3.925,6.79829941970784));
#46023=CARTESIAN_POINT('Origin',(0.5,-3.925,6.79829941970784));
#46024=CARTESIAN_POINT('',(9.,-3.90268918845559,6.98348173179481));
#46025=CARTESIAN_POINT('',(4.75,-3.90268918845559,6.98348173179481));
#46026=CARTESIAN_POINT('',(9.,-3.925,6.79829941970784));
#46027=CARTESIAN_POINT('Origin',(9.,-3.975,6.88490196008629));
#46028=CARTESIAN_POINT('Origin',(9.,0.,0.));
#46029=CARTESIAN_POINT('Origin',(0.5,-2.89421604688952,7.51322257582771));
#46030=CARTESIAN_POINT('',(9.,-2.84105711946744,7.47852889570692));
#46031=CARTESIAN_POINT('',(0.499999999999999,-2.84105711946744,7.47852889570692));
#46032=CARTESIAN_POINT('',(4.75,-2.84105711946744,7.47852889570692));
#46033=CARTESIAN_POINT('',(9.,-2.6848581251065,7.37658707316938));
#46034=CARTESIAN_POINT('',(9.,-2.89421604688952,7.51322257582771));
#46035=CARTESIAN_POINT('',(0.5,-2.6848581251065,7.37658707316938));
#46036=CARTESIAN_POINT('',(0.5,-2.6848581251065,7.37658707316938));
#46037=CARTESIAN_POINT('',(0.5,-2.89421604688952,7.51322257582771));
#46038=CARTESIAN_POINT('Origin',(0.5,-2.71906013943907,7.47055633524797));
#46039=CARTESIAN_POINT('',(0.499999999999999,-2.63072969389152,7.55508181806639));
#46040=CARTESIAN_POINT('Origin',(0.5,0.,0.));
#46041=CARTESIAN_POINT('',(0.5,-2.6848581251065,7.37658707316938));
#46042=CARTESIAN_POINT('Origin',(0.5,-2.6848581251065,7.37658707316938));
#46043=CARTESIAN_POINT('',(9.,-2.63072969389152,7.55508181806639));
#46044=CARTESIAN_POINT('',(4.75,-2.63072969389152,7.55508181806639));
#46045=CARTESIAN_POINT('',(9.,-2.6848581251065,7.37658707316938));
#46046=CARTESIAN_POINT('Origin',(9.,-2.71906013943907,7.47055633524797));
#46047=CARTESIAN_POINT('Origin',(9.,0.,0.));
#46048=CARTESIAN_POINT('Origin',(0.5,-1.54558899317062,7.90165518509824));
#46049=CARTESIAN_POINT('',(9.,-1.49926216363308,7.85825762906118));
#46050=CARTESIAN_POINT('',(0.499999999999999,-1.49926216363308,7.85825762906118));
#46051=CARTESIAN_POINT('',(4.75,-1.49926216363308,7.85825762906118));
#46052=CARTESIAN_POINT('',(9.,-1.3631381946854,7.73074086114583));
#46053=CARTESIAN_POINT('',(9.,-1.54558899317062,7.90165518509824));
#46054=CARTESIAN_POINT('',(0.5,-1.3631381946854,7.73074086114583));
#46055=CARTESIAN_POINT('',(0.5,-1.3631381946854,7.73074086114583));
#46056=CARTESIAN_POINT('',(0.5,-1.54558899317062,7.90165518509824));
#46057=CARTESIAN_POINT('Origin',(0.5,-1.3805030124521,7.82922163644705));
#46058=CARTESIAN_POINT('',(0.499999999999999,-1.27883680879202,7.8971245663519));
#46059=CARTESIAN_POINT('Origin',(0.5,0.,0.));
#46060=CARTESIAN_POINT('',(0.5,-1.3631381946854,7.73074086114583));
#46061=CARTESIAN_POINT('Origin',(0.5,-1.3631381946854,7.73074086114583));
#46062=CARTESIAN_POINT('',(9.,-1.27883680879202,7.8971245663519));
#46063=CARTESIAN_POINT('',(4.75,-1.27883680879202,7.8971245663519));
#46064=CARTESIAN_POINT('',(9.,-1.3631381946854,7.73074086114583));
#46065=CARTESIAN_POINT('Origin',(9.,-1.3805030124521,7.82922163644705));
#46066=CARTESIAN_POINT('Origin',(9.,0.,0.));
#46067=CARTESIAN_POINT('Origin',(0.5,-0.15,8.05));
#46068=CARTESIAN_POINT('',(9.,-0.111912885619985,7.99921718082665));
#46069=CARTESIAN_POINT('',(0.499999999999999,-0.111912885619985,7.99921718082665));
#46070=CARTESIAN_POINT('',(4.75,-0.111912885619985,7.99921718082665));
#46071=CARTESIAN_POINT('',(9.,4.80673868665336E-16,7.85));
#46072=CARTESIAN_POINT('',(9.,-0.15,8.05));
#46073=CARTESIAN_POINT('',(0.5,4.80673868665336E-16,7.85));
#46074=CARTESIAN_POINT('',(0.5,4.80673868665336E-16,7.85));
#46075=CARTESIAN_POINT('',(0.5,-0.15,8.05));
#46076=CARTESIAN_POINT('Origin',(0.5,4.86797102661073E-16,7.95));
#46077=CARTESIAN_POINT('',(0.499999999999999,0.111912885619987,7.99921718082665));
#46078=CARTESIAN_POINT('Origin',(0.5,0.,0.));
#46079=CARTESIAN_POINT('',(0.5,4.80673868665336E-16,7.85));
#46080=CARTESIAN_POINT('Origin',(0.5,4.80673868665336E-16,7.85));
#46081=CARTESIAN_POINT('',(9.,0.111912885619987,7.99921718082665));
#46082=CARTESIAN_POINT('',(4.75,0.111912885619987,7.99921718082665));
#46083=CARTESIAN_POINT('',(9.,4.80673868665336E-16,7.85));
#46084=CARTESIAN_POINT('Origin',(9.,4.86797102661073E-16,7.95));
#46085=CARTESIAN_POINT('Origin',(9.,0.,0.));
#46086=CARTESIAN_POINT('Origin',(0.5,1.25014666726696,7.95374963839832));
#46087=CARTESIAN_POINT('',(9.,1.27883680879202,7.8971245663519));
#46088=CARTESIAN_POINT('',(0.499999999999999,1.27883680879202,7.8971245663519));
#46089=CARTESIAN_POINT('',(4.75,1.27883680879202,7.8971245663519));
#46090=CARTESIAN_POINT('',(9.,1.3631381946854,7.73074086114583));
#46091=CARTESIAN_POINT('',(9.,1.25014666726696,7.95374963839832));
#46092=CARTESIAN_POINT('',(0.5,1.3631381946854,7.73074086114583));
#46093=CARTESIAN_POINT('',(0.5,1.3631381946854,7.73074086114583));
#46094=CARTESIAN_POINT('',(0.5,1.25014666726696,7.95374963839832));
#46095=CARTESIAN_POINT('Origin',(0.5,1.3805030124521,7.82922163644705));
#46096=CARTESIAN_POINT('',(0.499999999999999,1.49926216363308,7.85825762906118));
#46097=CARTESIAN_POINT('Origin',(0.5,0.,0.));
#46098=CARTESIAN_POINT('',(0.5,1.3631381946854,7.73074086114583));
#46099=CARTESIAN_POINT('Origin',(0.5,1.3631381946854,7.73074086114583));
#46100=CARTESIAN_POINT('',(9.,1.49926216363308,7.85825762906118));
#46101=CARTESIAN_POINT('',(4.75,1.49926216363308,7.85825762906118));
#46102=CARTESIAN_POINT('',(9.,1.3631381946854,7.73074086114583));
#46103=CARTESIAN_POINT('Origin',(9.,1.3805030124521,7.82922163644705));
#46104=CARTESIAN_POINT('Origin',(9.,0.,0.));
#46105=CARTESIAN_POINT('Origin',(0.5,2.61230826065375,7.61582861882541));
#46106=CARTESIAN_POINT('',(9.,2.63072969389153,7.55508181806639));
#46107=CARTESIAN_POINT('',(0.499999999999999,2.63072969389153,7.55508181806639));
#46108=CARTESIAN_POINT('',(4.75,2.63072969389153,7.55508181806639));
#46109=CARTESIAN_POINT('',(9.,2.6848581251065,7.37658707316938));
#46110=CARTESIAN_POINT('',(9.,2.61230826065375,7.61582861882541));
#46111=CARTESIAN_POINT('',(0.5,2.6848581251065,7.37658707316938));
#46112=CARTESIAN_POINT('',(0.5,2.6848581251065,7.37658707316938));
#46113=CARTESIAN_POINT('',(0.5,2.61230826065375,7.61582861882541));
#46114=CARTESIAN_POINT('Origin',(0.5,2.71906013943907,7.47055633524797));
#46115=CARTESIAN_POINT('',(0.499999999999999,2.84105711946744,7.47852889570692));
#46116=CARTESIAN_POINT('Origin',(0.5,0.,0.));
#46117=CARTESIAN_POINT('',(0.5,2.6848581251065,7.37658707316938));
#46118=CARTESIAN_POINT('Origin',(0.5,2.6848581251065,7.37658707316938));
#46119=CARTESIAN_POINT('',(9.,2.84105711946744,7.47852889570692));
#46120=CARTESIAN_POINT('',(4.75,2.84105711946744,7.47852889570692));
#46121=CARTESIAN_POINT('',(9.,2.6848581251065,7.37658707316938));
#46122=CARTESIAN_POINT('Origin',(9.,2.71906013943907,7.47055633524797));
#46123=CARTESIAN_POINT('Origin',(9.,0.,0.));
#46124=CARTESIAN_POINT('Origin',(0.5,3.89509618943234,7.04650450046473));
#46125=CARTESIAN_POINT('',(9.,3.9026891884556,6.98348173179481));
#46126=CARTESIAN_POINT('',(0.499999999999999,3.9026891884556,6.98348173179481));
#46127=CARTESIAN_POINT('',(4.75,3.9026891884556,6.98348173179481));
#46128=CARTESIAN_POINT('',(9.,3.925,6.79829941970784));
#46129=CARTESIAN_POINT('',(9.,3.89509618943234,7.04650450046473));
#46130=CARTESIAN_POINT('',(0.5,3.925,6.79829941970784));
#46131=CARTESIAN_POINT('',(0.5,3.925,6.79829941970784));
#46132=CARTESIAN_POINT('',(0.5,3.89509618943234,7.04650450046473));
#46133=CARTESIAN_POINT('Origin',(0.5,3.975,6.88490196008629));
#46134=CARTESIAN_POINT('',(0.499999999999999,4.09652799237105,6.87156884617482));
#46135=CARTESIAN_POINT('Origin',(0.5,0.,0.));
#46136=CARTESIAN_POINT('',(0.5,3.925,6.79829941970784));
#46137=CARTESIAN_POINT('Origin',(0.5,3.925,6.79829941970784));
#46138=CARTESIAN_POINT('',(9.,4.09652799237105,6.87156884617482));
#46139=CARTESIAN_POINT('',(4.75,4.09652799237105,6.87156884617482));
#46140=CARTESIAN_POINT('',(9.,3.925,6.79829941970784));
#46141=CARTESIAN_POINT('Origin',(9.,3.975,6.88490196008629));
#46142=CARTESIAN_POINT('Origin',(9.,0.,0.));
#46143=CARTESIAN_POINT('Origin',(0.5,5.0595335915088,6.26307590856075));
#46144=CARTESIAN_POINT('',(9.,5.05606744688446,6.1996920869149));
#46145=CARTESIAN_POINT('',(0.499999999999999,5.05606744688446,6.1996920869149));
#46146=CARTESIAN_POINT('',(4.75,5.05606744688446,6.1996920869149));
#46147=CARTESIAN_POINT('',(9.,5.04588273603933,6.01344887848398));
#46148=CARTESIAN_POINT('',(9.,5.0595335915088,6.26307590856075));
#46149=CARTESIAN_POINT('',(0.5,5.04588273603933,6.01344887848398));
#46150=CARTESIAN_POINT('',(0.5,5.04588273603933,6.01344887848398));
#46151=CARTESIAN_POINT('',(0.5,5.0595335915088,6.26307590856075));
#46152=CARTESIAN_POINT('Origin',(0.5,5.11016149700799,6.09005332279587));
#46153=CARTESIAN_POINT('',(0.499999999999999,5.22752793516966,6.05581965443332));
#46154=CARTESIAN_POINT('Origin',(0.5,0.,0.));
#46155=CARTESIAN_POINT('',(0.5,5.04588273603933,6.01344887848398));
#46156=CARTESIAN_POINT('Origin',(0.5,5.04588273603933,6.01344887848398));
#46157=CARTESIAN_POINT('',(9.,5.22752793516966,6.05581965443332));
#46158=CARTESIAN_POINT('',(4.75,5.22752793516966,6.05581965443332));
#46159=CARTESIAN_POINT('',(9.,5.04588273603933,6.01344887848398));
#46160=CARTESIAN_POINT('Origin',(9.,5.11016149700799,6.09005332279587));
#46161=CARTESIAN_POINT('Origin',(9.,0.,0.));
#46162=CARTESIAN_POINT('Origin',(0.5,6.07023962565479,5.28934692444449));
#46163=CARTESIAN_POINT('',(9.,6.05581965443332,5.22752793516966));
#46164=CARTESIAN_POINT('',(0.499999999999999,6.05581965443332,5.22752793516966));
#46165=CARTESIAN_POINT('',(4.75,6.05581965443332,5.22752793516966));
#46166=CARTESIAN_POINT('',(9.,6.01344887848398,5.04588273603933));
#46167=CARTESIAN_POINT('',(9.,6.07023962565479,5.28934692444449));
#46168=CARTESIAN_POINT('',(0.5,6.01344887848398,5.04588273603933));
#46169=CARTESIAN_POINT('',(0.5,6.01344887848398,5.04588273603933));
#46170=CARTESIAN_POINT('',(0.5,6.07023962565479,5.28934692444449));
#46171=CARTESIAN_POINT('Origin',(0.5,6.09005332279588,5.11016149700799));
#46172=CARTESIAN_POINT('',(0.499999999999999,6.1996920869149,5.05606744688446));
#46173=CARTESIAN_POINT('Origin',(0.5,0.,0.));
#46174=CARTESIAN_POINT('',(0.5,6.01344887848398,5.04588273603933));
#46175=CARTESIAN_POINT('Origin',(0.5,6.01344887848398,5.04588273603933));
#46176=CARTESIAN_POINT('',(9.,6.1996920869149,5.05606744688446));
#46177=CARTESIAN_POINT('',(4.75,6.1996920869149,5.05606744688446));
#46178=CARTESIAN_POINT('',(9.,6.01344887848398,5.04588273603933));
#46179=CARTESIAN_POINT('Origin',(9.,6.09005332279588,5.11016149700799));
#46180=CARTESIAN_POINT('Origin',(9.,0.,0.));
#46181=CARTESIAN_POINT('Origin',(0.5,6.89650450046473,4.15490381056767));
#46182=CARTESIAN_POINT('',(9.,6.87156884617482,4.09652799237105));
#46183=CARTESIAN_POINT('',(0.499999999999999,6.87156884617482,4.09652799237105));
#46184=CARTESIAN_POINT('',(4.75,6.87156884617482,4.09652799237105));
#46185=CARTESIAN_POINT('',(9.,6.79829941970784,3.925));
#46186=CARTESIAN_POINT('',(9.,6.89650450046473,4.15490381056767));
#46187=CARTESIAN_POINT('',(0.5,6.79829941970784,3.925));
#46188=CARTESIAN_POINT('',(0.5,6.79829941970784,3.925));
#46189=CARTESIAN_POINT('',(0.5,6.89650450046473,4.15490381056767));
#46190=CARTESIAN_POINT('Origin',(0.5,6.88490196008629,3.975));
#46191=CARTESIAN_POINT('',(0.499999999999999,6.98348173179481,3.90268918845559));
#46192=CARTESIAN_POINT('Origin',(0.5,0.,0.));
#46193=CARTESIAN_POINT('',(0.5,6.79829941970784,3.925));
#46194=CARTESIAN_POINT('Origin',(0.5,6.79829941970784,3.925));
#46195=CARTESIAN_POINT('',(9.,6.98348173179481,3.90268918845559));
#46196=CARTESIAN_POINT('',(4.75,6.98348173179481,3.90268918845559));
#46197=CARTESIAN_POINT('',(9.,6.79829941970784,3.925));
#46198=CARTESIAN_POINT('Origin',(9.,6.88490196008629,3.975));
#46199=CARTESIAN_POINT('Origin',(9.,0.,0.));
#46200=CARTESIAN_POINT('Origin',(0.5,7.51322257582771,2.89421604688952));
#46201=CARTESIAN_POINT('',(9.,7.47852889570692,2.84105711946744));
#46202=CARTESIAN_POINT('',(0.499999999999999,7.47852889570692,2.84105711946744));
#46203=CARTESIAN_POINT('',(4.75,7.47852889570692,2.84105711946744));
#46204=CARTESIAN_POINT('',(9.,7.37658707316938,2.6848581251065));
#46205=CARTESIAN_POINT('',(9.,7.51322257582771,2.89421604688952));
#46206=CARTESIAN_POINT('',(0.5,7.37658707316938,2.6848581251065));
#46207=CARTESIAN_POINT('',(0.5,7.37658707316938,2.6848581251065));
#46208=CARTESIAN_POINT('',(0.5,7.51322257582771,2.89421604688952));
#46209=CARTESIAN_POINT('Origin',(0.5,7.47055633524797,2.71906013943907));
#46210=CARTESIAN_POINT('',(0.499999999999999,7.55508181806639,2.63072969389152));
#46211=CARTESIAN_POINT('Origin',(0.5,0.,0.));
#46212=CARTESIAN_POINT('',(0.5,7.37658707316938,2.6848581251065));
#46213=CARTESIAN_POINT('Origin',(0.5,7.37658707316938,2.6848581251065));
#46214=CARTESIAN_POINT('',(9.,7.55508181806639,2.63072969389152));
#46215=CARTESIAN_POINT('',(4.75,7.55508181806639,2.63072969389152));
#46216=CARTESIAN_POINT('',(9.,7.37658707316938,2.6848581251065));
#46217=CARTESIAN_POINT('Origin',(9.,7.47055633524797,2.71906013943907));
#46218=CARTESIAN_POINT('Origin',(9.,0.,0.));
#46219=CARTESIAN_POINT('Origin',(0.5,7.90165518509824,1.54558899317062));
#46220=CARTESIAN_POINT('',(9.,7.85825762906118,1.49926216363308));
#46221=CARTESIAN_POINT('',(0.499999999999999,7.85825762906118,1.49926216363308));
#46222=CARTESIAN_POINT('',(4.75,7.85825762906118,1.49926216363308));
#46223=CARTESIAN_POINT('',(9.,7.73074086114583,1.3631381946854));
#46224=CARTESIAN_POINT('',(9.,7.90165518509824,1.54558899317062));
#46225=CARTESIAN_POINT('',(0.5,7.73074086114583,1.3631381946854));
#46226=CARTESIAN_POINT('',(0.5,7.73074086114583,1.3631381946854));
#46227=CARTESIAN_POINT('',(0.5,7.90165518509824,1.54558899317062));
#46228=CARTESIAN_POINT('Origin',(0.5,7.82922163644705,1.3805030124521));
#46229=CARTESIAN_POINT('',(0.499999999999999,7.8971245663519,1.27883680879202));
#46230=CARTESIAN_POINT('Origin',(0.5,0.,0.));
#46231=CARTESIAN_POINT('',(0.5,7.73074086114583,1.3631381946854));
#46232=CARTESIAN_POINT('Origin',(0.5,7.73074086114583,1.3631381946854));
#46233=CARTESIAN_POINT('',(9.,7.8971245663519,1.27883680879202));
#46234=CARTESIAN_POINT('',(4.75,7.8971245663519,1.27883680879202));
#46235=CARTESIAN_POINT('',(9.,7.73074086114583,1.3631381946854));
#46236=CARTESIAN_POINT('Origin',(9.,7.82922163644705,1.3805030124521));
#46237=CARTESIAN_POINT('Origin',(9.,0.,0.));
#46238=CARTESIAN_POINT('Origin',(0.5,8.05,0.15));
#46239=CARTESIAN_POINT('',(9.,7.99921718082665,0.111912885619985));
#46240=CARTESIAN_POINT('',(0.499999999999999,7.99921718082665,0.111912885619985));
#46241=CARTESIAN_POINT('',(4.75,7.99921718082665,0.111912885619985));
#46242=CARTESIAN_POINT('',(9.,7.85,0.));
#46243=CARTESIAN_POINT('',(9.,8.05,0.15));
#46244=CARTESIAN_POINT('',(0.5,7.85,0.));
#46245=CARTESIAN_POINT('',(0.5,7.85,0.));
#46246=CARTESIAN_POINT('',(0.5,8.05,0.15));
#46247=CARTESIAN_POINT('Origin',(0.5,7.95,0.));
#46248=CARTESIAN_POINT('',(0.499999999999999,7.99921718082665,-0.111912885619987));
#46249=CARTESIAN_POINT('Origin',(0.5,0.,0.));
#46250=CARTESIAN_POINT('',(0.5,7.85,0.));
#46251=CARTESIAN_POINT('Origin',(0.5,7.85,0.));
#46252=CARTESIAN_POINT('',(9.,7.99921718082665,-0.111912885619987));
#46253=CARTESIAN_POINT('',(4.75,7.99921718082665,-0.111912885619987));
#46254=CARTESIAN_POINT('',(9.,7.85,0.));
#46255=CARTESIAN_POINT('Origin',(9.,7.95,0.));
#46256=CARTESIAN_POINT('Origin',(9.,0.,0.));
#46257=CARTESIAN_POINT('Origin',(10.,5.55111512312578E-16,4.61880215351701));
#46258=CARTESIAN_POINT('',(10.,2.82820063659975E-16,4.61880215351701));
#46259=CARTESIAN_POINT('',(10.,4.,2.3094010767585));
#46260=CARTESIAN_POINT('',(10.,1.,4.04145188432738));
#46261=CARTESIAN_POINT('',(5.,5.55111512312578E-16,4.61880215351701));
#46262=CARTESIAN_POINT('',(10.,2.82820063659975E-16,4.61880215351701));
#46263=CARTESIAN_POINT('',(5.,4.,2.3094010767585));
#46264=CARTESIAN_POINT('',(5.,4.,2.3094010767585));
#46265=CARTESIAN_POINT('',(10.,4.,2.3094010767585));
#46266=CARTESIAN_POINT('Origin',(10.,-4.,2.3094010767585));
#46267=CARTESIAN_POINT('',(10.,-4.,2.3094010767585));
#46268=CARTESIAN_POINT('',(10.,-3.,2.88675134594813));
#46269=CARTESIAN_POINT('',(5.,-4.,2.3094010767585));
#46270=CARTESIAN_POINT('',(10.,-4.,2.3094010767585));
#46271=CARTESIAN_POINT('',(5.,2.82820063659975E-16,4.61880215351701));
#46272=CARTESIAN_POINT('Origin',(10.,-4.,-2.3094010767585));
#46273=CARTESIAN_POINT('',(10.,-4.,-2.3094010767585));
#46274=CARTESIAN_POINT('',(10.,-4.,-1.15470053837925));
#46275=CARTESIAN_POINT('',(5.,-4.,-2.3094010767585));
#46276=CARTESIAN_POINT('',(10.,-4.,-2.3094010767585));
#46277=CARTESIAN_POINT('',(5.,-4.,2.3094010767585));
#46278=CARTESIAN_POINT('Origin',(10.,-1.11022302462516E-15,-4.61880215351701));
#46279=CARTESIAN_POINT('',(10.,-8.48460190979926E-16,-4.61880215351701));
#46280=CARTESIAN_POINT('',(10.,-1.,-4.04145188432738));
#46281=CARTESIAN_POINT('',(5.,-1.11022302462516E-15,-4.61880215351701));
#46282=CARTESIAN_POINT('',(10.,-8.48460190979926E-16,-4.61880215351701));
#46283=CARTESIAN_POINT('',(5.,-4.,-2.3094010767585));
#46284=CARTESIAN_POINT('Origin',(10.,4.,-2.30940107675851));
#46285=CARTESIAN_POINT('',(10.,4.,-2.30940107675851));
#46286=CARTESIAN_POINT('',(10.,3.,-2.88675134594813));
#46287=CARTESIAN_POINT('',(5.,4.,-2.30940107675851));
#46288=CARTESIAN_POINT('',(10.,4.,-2.30940107675851));
#46289=CARTESIAN_POINT('',(5.,-8.48460190979926E-16,-4.61880215351701));
#46290=CARTESIAN_POINT('Origin',(10.,4.,2.3094010767585));
#46291=CARTESIAN_POINT('',(10.,4.,1.15470053837925));
#46292=CARTESIAN_POINT('',(5.,4.,-2.30940107675851));
#46293=CARTESIAN_POINT('Origin',(5.,0.,0.));
#46294=CARTESIAN_POINT('Origin',(-90.,4.5,0.));
#46295=CARTESIAN_POINT('',(-90.,-4.5,-5.51091059616309E-16));
#46296=CARTESIAN_POINT('Origin',(-90.,0.,0.));
#46297=CARTESIAN_POINT('Origin',(-89.75,0.,0.));
#46298=CARTESIAN_POINT('',(-89.75,-4.75,-5.81707229594993E-16));
#46299=CARTESIAN_POINT('Origin',(-74.75,0.,0.));
#46300=CARTESIAN_POINT('Origin',(-59.25,0.,0.));
#46301=CARTESIAN_POINT('Origin',(-59.75,0.,0.));
#46302=CARTESIAN_POINT('',(-59.5,-4.95,-6.0620016557794E-16));
#46303=CARTESIAN_POINT('Origin',(-59.5,0.,0.));
#46304=CARTESIAN_POINT('',(-59.75,-4.975,-6.09261782575808E-16));
#46305=CARTESIAN_POINT('Origin',(-29.75,0.,0.));
#46306=CARTESIAN_POINT('',(0.,-4.95,-6.0620016557794E-16));
#46307=CARTESIAN_POINT('Origin',(0.,0.,0.));
#46308=CARTESIAN_POINT('',(-29.75,-4.95,-6.0620016557794E-16));
#46309=CARTESIAN_POINT('Origin',(0.,8.,0.));
#46310=CARTESIAN_POINT('',(5.55111512312578E-16,-8.,-9.79717439317883E-16));
#46311=CARTESIAN_POINT('Origin',(0.,0.,0.));
#46312=CARTESIAN_POINT('Origin',(4.75,0.,0.));
#46313=CARTESIAN_POINT('',(9.5,-8.,-9.79717439317883E-16));
#46314=CARTESIAN_POINT('Origin',(9.5,0.,0.));
#46315=CARTESIAN_POINT('',(4.75,-8.,-9.79717439317883E-16));
#46316=CARTESIAN_POINT('',(4.75,-8.,-9.79717439317883E-16));
#46317=CARTESIAN_POINT('Origin',(9.75,0.,0.));
#46318=CARTESIAN_POINT('',(10.,-7.5,-9.18485099360515E-16));
#46319=CARTESIAN_POINT('Origin',(10.,0.,0.));
#46320=CARTESIAN_POINT('',(9.75,-7.75,-9.49101269339199E-16));
#46321=CARTESIAN_POINT('Origin',(10.,0.,0.));
#46322=CARTESIAN_POINT('',(0.,0.,0.));
#46323=CARTESIAN_POINT('Origin',(0.,3.6,0.));
#46324=CARTESIAN_POINT('',(3.46944695195361E-17,-3.6,-4.40872847693047E-16));
#46325=CARTESIAN_POINT('Origin',(0.,0.,0.));
#46326=CARTESIAN_POINT('Origin',(0.2,0.,0.));
#46327=CARTESIAN_POINT('',(0.4,-4.,-4.89858719658941E-16));
#46328=CARTESIAN_POINT('Origin',(0.4,0.,0.));
#46329=CARTESIAN_POINT('',(0.2,-3.8,-4.65365783675994E-16));
#46330=CARTESIAN_POINT('Origin',(8.,0.,0.));
#46331=CARTESIAN_POINT('',(15.6,-4.,-4.89858719658941E-16));
#46332=CARTESIAN_POINT('Origin',(15.6,0.,0.));
#46333=CARTESIAN_POINT('',(8.,-4.,-4.89858719658941E-16));
#46334=CARTESIAN_POINT('Origin',(15.8,0.,0.));
#46335=CARTESIAN_POINT('',(16.,-3.6,-4.40872847693047E-16));
#46336=CARTESIAN_POINT('Origin',(16.,0.,0.));
#46337=CARTESIAN_POINT('',(15.8,-3.8,-4.65365783675994E-16));
#46338=CARTESIAN_POINT('Origin',(16.,0.,0.));
#46339=CARTESIAN_POINT('',(0.,0.,0.));
#46340=CARTESIAN_POINT('',(0.,0.,0.));
#46341=CARTESIAN_POINT('',(0.,0.,0.));
#46342=CARTESIAN_POINT('',(0.,0.,0.));
#46343=CARTESIAN_POINT('',(0.,0.,0.));
#46344=CARTESIAN_POINT('',(0.,0.,0.));
#46345=CARTESIAN_POINT('',(0.,102.,0.));
#46346=CARTESIAN_POINT('',(0.,-4.25,0.));
#46347=CARTESIAN_POINT('',(0.,-5.45,0.));
#46348=CARTESIAN_POINT('',(0.,0.,0.));
#46349=CARTESIAN_POINT('',(0.,0.,0.));
#46350=CARTESIAN_POINT('',(0.,102.,0.));
#46351=CARTESIAN_POINT('',(0.,105.7,-16.5));
#46352=CARTESIAN_POINT('',(0.,19.5,0.));
#46353=CARTESIAN_POINT('',(0.,19.5,-33.));
#46354=CARTESIAN_POINT('',(0.,66.5,0.));
#46355=CARTESIAN_POINT('',(0.,66.5,-33.));
#46356=CARTESIAN_POINT('',(30.5,93.7,22.));
#46357=CARTESIAN_POINT('',(-30.5,93.7,22.));
#46358=CARTESIAN_POINT('',(30.5,93.7,-55.));
#46359=CARTESIAN_POINT('',(-30.5,93.7,-55.));
#46360=CARTESIAN_POINT('',(30.5,10.05,-16.5));
#46361=CARTESIAN_POINT('',(30.5,75.95,-16.5));
#46362=CARTESIAN_POINT('',(-30.5,10.05,-16.5));
#46363=CARTESIAN_POINT('',(-30.5,75.95,-16.5));
#46364=UNCERTAINTY_MEASURE_WITH_UNIT(LENGTH_MEASURE(0.01),#46396,
'DISTANCE_ACCURACY_VALUE',
'Maximum model space distance between geometric entities at asserted c
onnectivities');
#46365=UNCERTAINTY_MEASURE_WITH_UNIT(LENGTH_MEASURE(0.01),#46396,
'DISTANCE_ACCURACY_VALUE',
'Maximum model space distance between geometric entities at asserted c
onnectivities');
#46366=UNCERTAINTY_MEASURE_WITH_UNIT(LENGTH_MEASURE(0.01),#46396,
'DISTANCE_ACCURACY_VALUE',
'Maximum model space distance between geometric entities at asserted c
onnectivities');
#46367=UNCERTAINTY_MEASURE_WITH_UNIT(LENGTH_MEASURE(0.01),#46396,
'DISTANCE_ACCURACY_VALUE',
'Maximum model space distance between geometric entities at asserted c
onnectivities');
#46368=UNCERTAINTY_MEASURE_WITH_UNIT(LENGTH_MEASURE(0.01),#46396,
'DISTANCE_ACCURACY_VALUE',
'Maximum model space distance between geometric entities at asserted c
onnectivities');
#46369=UNCERTAINTY_MEASURE_WITH_UNIT(LENGTH_MEASURE(0.01),#46396,
'DISTANCE_ACCURACY_VALUE',
'Maximum model space distance between geometric entities at asserted c
onnectivities');
#46370=UNCERTAINTY_MEASURE_WITH_UNIT(LENGTH_MEASURE(0.01),#46396,
'DISTANCE_ACCURACY_VALUE',
'Maximum model space distance between geometric entities at asserted c
onnectivities');
#46371=UNCERTAINTY_MEASURE_WITH_UNIT(LENGTH_MEASURE(0.01),#46396,
'DISTANCE_ACCURACY_VALUE',
'Maximum model space distance between geometric entities at asserted c
onnectivities');
#46372=UNCERTAINTY_MEASURE_WITH_UNIT(LENGTH_MEASURE(0.01),#46396,
'DISTANCE_ACCURACY_VALUE',
'Maximum model space distance between geometric entities at asserted c
onnectivities');
#46373=UNCERTAINTY_MEASURE_WITH_UNIT(LENGTH_MEASURE(0.01),#46396,
'DISTANCE_ACCURACY_VALUE',
'Maximum model space distance between geometric entities at asserted c
onnectivities');
#46374=UNCERTAINTY_MEASURE_WITH_UNIT(LENGTH_MEASURE(0.01),#46396,
'DISTANCE_ACCURACY_VALUE',
'Maximum model space distance between geometric entities at asserted c
onnectivities');
#46375=UNCERTAINTY_MEASURE_WITH_UNIT(LENGTH_MEASURE(0.01),#46396,
'DISTANCE_ACCURACY_VALUE',
'Maximum model space distance between geometric entities at asserted c
onnectivities');
#46376=UNCERTAINTY_MEASURE_WITH_UNIT(LENGTH_MEASURE(0.01),#46396,
'DISTANCE_ACCURACY_VALUE',
'Maximum model space distance between geometric entities at asserted c
onnectivities');
#46377=UNCERTAINTY_MEASURE_WITH_UNIT(LENGTH_MEASURE(0.01),#46396,
'DISTANCE_ACCURACY_VALUE',
'Maximum model space distance between geometric entities at asserted c
onnectivities');
#46378=UNCERTAINTY_MEASURE_WITH_UNIT(LENGTH_MEASURE(0.01),#46396,
'DISTANCE_ACCURACY_VALUE',
'Maximum model space distance between geometric entities at asserted c
onnectivities');
#46379=UNCERTAINTY_MEASURE_WITH_UNIT(LENGTH_MEASURE(0.01),#46396,
'DISTANCE_ACCURACY_VALUE',
'Maximum model space distance between geometric entities at asserted c
onnectivities');
#46380=(
GEOMETRIC_REPRESENTATION_CONTEXT(3)
GLOBAL_UNCERTAINTY_ASSIGNED_CONTEXT((#46364))
GLOBAL_UNIT_ASSIGNED_CONTEXT((#46396,#46398,#46399))
REPRESENTATION_CONTEXT('','3D')
);
#46381=(
GEOMETRIC_REPRESENTATION_CONTEXT(3)
GLOBAL_UNCERTAINTY_ASSIGNED_CONTEXT((#46365))
GLOBAL_UNIT_ASSIGNED_CONTEXT((#46396,#46398,#46399))
REPRESENTATION_CONTEXT('','3D')
);
#46382=(
GEOMETRIC_REPRESENTATION_CONTEXT(3)
GLOBAL_UNCERTAINTY_ASSIGNED_CONTEXT((#46366))
GLOBAL_UNIT_ASSIGNED_CONTEXT((#46396,#46398,#46399))
REPRESENTATION_CONTEXT('','3D')
);
#46383=(
GEOMETRIC_REPRESENTATION_CONTEXT(3)
GLOBAL_UNCERTAINTY_ASSIGNED_CONTEXT((#46367))
GLOBAL_UNIT_ASSIGNED_CONTEXT((#46396,#46398,#46399))
REPRESENTATION_CONTEXT('','3D')
);
#46384=(
GEOMETRIC_REPRESENTATION_CONTEXT(3)
GLOBAL_UNCERTAINTY_ASSIGNED_CONTEXT((#46368))
GLOBAL_UNIT_ASSIGNED_CONTEXT((#46396,#46398,#46399))
REPRESENTATION_CONTEXT('','3D')
);
#46385=(
GEOMETRIC_REPRESENTATION_CONTEXT(3)
GLOBAL_UNCERTAINTY_ASSIGNED_CONTEXT((#46369))
GLOBAL_UNIT_ASSIGNED_CONTEXT((#46396,#46398,#46399))
REPRESENTATION_CONTEXT('','3D')
);
#46386=(
GEOMETRIC_REPRESENTATION_CONTEXT(3)
GLOBAL_UNCERTAINTY_ASSIGNED_CONTEXT((#46370))
GLOBAL_UNIT_ASSIGNED_CONTEXT((#46396,#46398,#46399))
REPRESENTATION_CONTEXT('','3D')
);
#46387=(
GEOMETRIC_REPRESENTATION_CONTEXT(3)
GLOBAL_UNCERTAINTY_ASSIGNED_CONTEXT((#46371))
GLOBAL_UNIT_ASSIGNED_CONTEXT((#46396,#46398,#46399))
REPRESENTATION_CONTEXT('','3D')
);
#46388=(
GEOMETRIC_REPRESENTATION_CONTEXT(3)
GLOBAL_UNCERTAINTY_ASSIGNED_CONTEXT((#46372))
GLOBAL_UNIT_ASSIGNED_CONTEXT((#46396,#46398,#46399))
REPRESENTATION_CONTEXT('','3D')
);
#46389=(
GEOMETRIC_REPRESENTATION_CONTEXT(3)
GLOBAL_UNCERTAINTY_ASSIGNED_CONTEXT((#46373))
GLOBAL_UNIT_ASSIGNED_CONTEXT((#46396,#46398,#46399))
REPRESENTATION_CONTEXT('','3D')
);
#46390=(
GEOMETRIC_REPRESENTATION_CONTEXT(3)
GLOBAL_UNCERTAINTY_ASSIGNED_CONTEXT((#46374))
GLOBAL_UNIT_ASSIGNED_CONTEXT((#46396,#46398,#46399))
REPRESENTATION_CONTEXT('','3D')
);
#46391=(
GEOMETRIC_REPRESENTATION_CONTEXT(3)
GLOBAL_UNCERTAINTY_ASSIGNED_CONTEXT((#46375))
GLOBAL_UNIT_ASSIGNED_CONTEXT((#46396,#46398,#46399))
REPRESENTATION_CONTEXT('','3D')
);
#46392=(
GEOMETRIC_REPRESENTATION_CONTEXT(3)
GLOBAL_UNCERTAINTY_ASSIGNED_CONTEXT((#46376))
GLOBAL_UNIT_ASSIGNED_CONTEXT((#46396,#46398,#46399))
REPRESENTATION_CONTEXT('','3D')
);
#46393=(
GEOMETRIC_REPRESENTATION_CONTEXT(3)
GLOBAL_UNCERTAINTY_ASSIGNED_CONTEXT((#46377))
GLOBAL_UNIT_ASSIGNED_CONTEXT((#46396,#46398,#46399))
REPRESENTATION_CONTEXT('','3D')
);
#46394=(
GEOMETRIC_REPRESENTATION_CONTEXT(3)
GLOBAL_UNCERTAINTY_ASSIGNED_CONTEXT((#46378))
GLOBAL_UNIT_ASSIGNED_CONTEXT((#46396,#46398,#46399))
REPRESENTATION_CONTEXT('','3D')
);
#46395=(
GEOMETRIC_REPRESENTATION_CONTEXT(3)
GLOBAL_UNCERTAINTY_ASSIGNED_CONTEXT((#46379))
GLOBAL_UNIT_ASSIGNED_CONTEXT((#46396,#46398,#46399))
REPRESENTATION_CONTEXT('','3D')
);
#46396=(
LENGTH_UNIT()
NAMED_UNIT(*)
SI_UNIT(.MILLI.,.METRE.)
);
#46397=(
LENGTH_UNIT()
NAMED_UNIT(*)
SI_UNIT($,.METRE.)
);
#46398=(
NAMED_UNIT(*)
PLANE_ANGLE_UNIT()
SI_UNIT($,.RADIAN.)
);
#46399=(
NAMED_UNIT(*)
SI_UNIT($,.STERADIAN.)
SOLID_ANGLE_UNIT()
);
#46400=SHAPE_DEFINITION_REPRESENTATION(#46415,#46455);
#46401=SHAPE_DEFINITION_REPRESENTATION(#46416,#46456);
#46402=SHAPE_DEFINITION_REPRESENTATION(#46417,#46457);
#46403=SHAPE_DEFINITION_REPRESENTATION(#46418,#46458);
#46404=SHAPE_DEFINITION_REPRESENTATION(#46419,#46459);
#46405=SHAPE_DEFINITION_REPRESENTATION(#46420,#46460);
#46406=SHAPE_DEFINITION_REPRESENTATION(#46421,#46461);
#46407=SHAPE_DEFINITION_REPRESENTATION(#46422,#46462);
#46408=SHAPE_DEFINITION_REPRESENTATION(#46423,#46463);
#46409=SHAPE_DEFINITION_REPRESENTATION(#46424,#46464);
#46410=SHAPE_DEFINITION_REPRESENTATION(#46425,#46465);
#46411=SHAPE_DEFINITION_REPRESENTATION(#46426,#46466);
#46412=SHAPE_DEFINITION_REPRESENTATION(#46427,#46467);
#46413=SHAPE_DEFINITION_REPRESENTATION(#46428,#46468);
#46414=SHAPE_DEFINITION_REPRESENTATION(#46429,#46469);
#46415=PRODUCT_DEFINITION_SHAPE('',$,#46471);
#46416=PRODUCT_DEFINITION_SHAPE('',$,#46472);
#46417=PRODUCT_DEFINITION_SHAPE('',$,#46473);
#46418=PRODUCT_DEFINITION_SHAPE('',$,#46474);
#46419=PRODUCT_DEFINITION_SHAPE('',$,#46475);
#46420=PRODUCT_DEFINITION_SHAPE('',$,#46476);
#46421=PRODUCT_DEFINITION_SHAPE('',$,#46477);
#46422=PRODUCT_DEFINITION_SHAPE('',$,#46478);
#46423=PRODUCT_DEFINITION_SHAPE('',$,#46479);
#46424=PRODUCT_DEFINITION_SHAPE('',$,#46480);
#46425=PRODUCT_DEFINITION_SHAPE('',$,#46481);
#46426=PRODUCT_DEFINITION_SHAPE('',$,#46482);
#46427=PRODUCT_DEFINITION_SHAPE('',$,#46483);
#46428=PRODUCT_DEFINITION_SHAPE('',$,#46484);
#46429=PRODUCT_DEFINITION_SHAPE('',$,#46485);
#46430=PRODUCT_DEFINITION_SHAPE($,$,#86);
#46431=PRODUCT_DEFINITION_SHAPE($,$,#87);
#46432=PRODUCT_DEFINITION_SHAPE($,$,#88);
#46433=PRODUCT_DEFINITION_SHAPE($,$,#89);
#46434=PRODUCT_DEFINITION_SHAPE($,$,#90);
#46435=PRODUCT_DEFINITION_SHAPE($,$,#91);
#46436=PRODUCT_DEFINITION_SHAPE($,$,#92);
#46437=PRODUCT_DEFINITION_SHAPE($,$,#93);
#46438=PRODUCT_DEFINITION_SHAPE($,$,#94);
#46439=PRODUCT_DEFINITION_SHAPE($,$,#95);
#46440=PRODUCT_DEFINITION_SHAPE($,$,#96);
#46441=PRODUCT_DEFINITION_SHAPE($,$,#97);
#46442=PRODUCT_DEFINITION_SHAPE($,$,#98);
#46443=PRODUCT_DEFINITION_SHAPE($,$,#99);
#46444=PRODUCT_DEFINITION_SHAPE($,$,#100);
#46445=PRODUCT_DEFINITION_SHAPE($,$,#101);
#46446=PRODUCT_DEFINITION_SHAPE($,$,#102);
#46447=PRODUCT_DEFINITION_SHAPE($,$,#103);
#46448=PRODUCT_DEFINITION_SHAPE($,$,#104);
#46449=PRODUCT_DEFINITION_SHAPE($,$,#105);
#46450=PRODUCT_DEFINITION_SHAPE($,$,#106);
#46451=PRODUCT_DEFINITION_SHAPE($,$,#107);
#46452=PRODUCT_DEFINITION_SHAPE($,$,#108);
#46453=PRODUCT_DEFINITION_SHAPE($,$,#109);
#46454=PRODUCT_DEFINITION_SHAPE($,$,#110);
#46455=SHAPE_REPRESENTATION('',(#25106,#26908,#26909,#26910,#26911,#26912,
#26913,#26914,#26915,#26916,#26917,#26918,#26919,#26920,#26921,#26922,#26923,
#26924,#26925,#26926,#26927,#26928,#26929,#26930,#26931,#26932),#46380);
#46456=SHAPE_REPRESENTATION('',(#25107),#46381);
#46457=SHAPE_REPRESENTATION('',(#25445),#46382);
#46458=SHAPE_REPRESENTATION('',(#25562),#46383);
#46459=SHAPE_REPRESENTATION('',(#25703),#46384);
#46460=SHAPE_REPRESENTATION('',(#26063),#46385);
#46461=SHAPE_REPRESENTATION('',(#26410),#46386);
#46462=SHAPE_REPRESENTATION('',(#26435),#46387);
#46463=SHAPE_REPRESENTATION('',(#26457),#46388);
#46464=SHAPE_REPRESENTATION('',(#26494),#46389);
#46465=SHAPE_REPRESENTATION('',(#26513),#46390);
#46466=SHAPE_REPRESENTATION('',(#26528),#46391);
#46467=SHAPE_REPRESENTATION('',(#26580),#46392);
#46468=SHAPE_REPRESENTATION('',(#26605),#46393);
#46469=SHAPE_REPRESENTATION('',(#26898),#46394);
#46470=PRODUCT_DEFINITION_CONTEXT('part definition',#46517,'design');
#46471=PRODUCT_DEFINITION('2026-10-26-00-50-37-162','MAS-346',#46486,#46470);
#46472=PRODUCT_DEFINITION('2026-10-26-00-50-38-164',
'01_Front_Flange_SAE_A',#46487,#46470);
#46473=PRODUCT_DEFINITION('2026-10-26-00-50-40-883','02_Gear_Body',#46488,
#46470);
#46474=PRODUCT_DEFINITION('2026-10-26-00-50-44-377','03_Rear_Cover',#46489,
#46470);
#46475=PRODUCT_DEFINITION('2026-10-26-00-50-47-232',
'04_Drive_Gear_Shaft_z12_m2.75',#46490,#46470);
#46476=PRODUCT_DEFINITION('2026-10-26-00-50-58-441',
'05_Driven_Gear_Shaft_z12_m2.75',#46491,#46470);
#46477=PRODUCT_DEFINITION('2026-10-26-00-51-10-414',
'06_Bearing_Block_Bronze',#46492,#46470);
#46478=PRODUCT_DEFINITION('2026-10-26-00-51-13-026',
'08_Shaft_Lip_Seal_5-8x1-1-8',#46493,#46470);
#46479=PRODUCT_DEFINITION('2026-10-26-00-51-13-699',
'09_Circlip_DIN_472_-_28',#46494,#46470);
#46480=PRODUCT_DEFINITION('2026-10-26-00-51-14-660','10_Shaft_Key_5-32',
#46495,#46470);
#46481=PRODUCT_DEFINITION('2026-10-26-00-51-15-440',
'11_Body_Face_Seal_O-Ring',#46496,#46470);
#46482=PRODUCT_DEFINITION('2026-10-26-00-51-20-172',
'14_Case_Drain_Plug_9-16-18',#46497,#46470);
#46483=PRODUCT_DEFINITION('2026-10-26-00-51-12-008',
'07_Needle_Bearing_HK1716_Drawn_Cup',#46498,#46470);
#46484=PRODUCT_DEFINITION('2026-10-26-00-51-16-707',
'12_Through_Bolt_ISO_4762_M10x90',#46499,#46470);
#46485=PRODUCT_DEFINITION('2026-10-26-00-51-19-479',
'13_Dowel_Pin_ISO_8734_8x16',#46500,#46470);
#46486=PRODUCT_DEFINITION_FORMATION('',$,#46519);
#46487=PRODUCT_DEFINITION_FORMATION('',$,#46520);
#46488=PRODUCT_DEFINITION_FORMATION('',$,#46521);
#46489=PRODUCT_DEFINITION_FORMATION('',$,#46522);
#46490=PRODUCT_DEFINITION_FORMATION('',$,#46523);
#46491=PRODUCT_DEFINITION_FORMATION('',$,#46524);
#46492=PRODUCT_DEFINITION_FORMATION('',$,#46525);
#46493=PRODUCT_DEFINITION_FORMATION('',$,#46526);
#46494=PRODUCT_DEFINITION_FORMATION('',$,#46527);
#46495=PRODUCT_DEFINITION_FORMATION('',$,#46528);
#46496=PRODUCT_DEFINITION_FORMATION('',$,#46529);
#46497=PRODUCT_DEFINITION_FORMATION('',$,#46530);
#46498=PRODUCT_DEFINITION_FORMATION('',$,#46531);
#46499=PRODUCT_DEFINITION_FORMATION('',$,#46532);
#46500=PRODUCT_DEFINITION_FORMATION('',$,#46533);
#46501=PRODUCT_RELATED_PRODUCT_CATEGORY('MAS-346','MAS-346',(#46519));
#46502=PRODUCT_RELATED_PRODUCT_CATEGORY('01_Front_Flange_SAE_A',
'01_Front_Flange_SAE_A',(#46520));
#46503=PRODUCT_RELATED_PRODUCT_CATEGORY('02_Gear_Body','02_Gear_Body',(#46521));
#46504=PRODUCT_RELATED_PRODUCT_CATEGORY('03_Rear_Cover','03_Rear_Cover',
(#46522));
#46505=PRODUCT_RELATED_PRODUCT_CATEGORY('04_Drive_Gear_Shaft_z12_m2.75',
'04_Drive_Gear_Shaft_z12_m2.75',(#46523));
#46506=PRODUCT_RELATED_PRODUCT_CATEGORY(
'05_Driven_Gear_Shaft_z12_m2.75','05_Driven_Gear_Shaft_z12_m2.75',(#46524));
#46507=PRODUCT_RELATED_PRODUCT_CATEGORY('06_Bearing_Block_Bronze',
'06_Bearing_Block_Bronze',(#46525));
#46508=PRODUCT_RELATED_PRODUCT_CATEGORY('08_Shaft_Lip_Seal_5-8x1-1-8',
'08_Shaft_Lip_Seal_5-8x1-1-8',(#46526));
#46509=PRODUCT_RELATED_PRODUCT_CATEGORY('09_Circlip_DIN_472_-_28',
'09_Circlip_DIN_472_-_28',(#46527));
#46510=PRODUCT_RELATED_PRODUCT_CATEGORY('10_Shaft_Key_5-32',
'10_Shaft_Key_5-32',(#46528));
#46511=PRODUCT_RELATED_PRODUCT_CATEGORY('11_Body_Face_Seal_O-Ring',
'11_Body_Face_Seal_O-Ring',(#46529));
#46512=PRODUCT_RELATED_PRODUCT_CATEGORY('14_Case_Drain_Plug_9-16-18',
'14_Case_Drain_Plug_9-16-18',(#46530));
#46513=PRODUCT_RELATED_PRODUCT_CATEGORY(
'07_Needle_Bearing_HK1716_Drawn_Cup',
'07_Needle_Bearing_HK1716_Drawn_Cup',(#46531));
#46514=PRODUCT_RELATED_PRODUCT_CATEGORY(
'12_Through_Bolt_ISO_4762_M10x90','12_Through_Bolt_ISO_4762_M10x90',(#46532));
#46515=PRODUCT_RELATED_PRODUCT_CATEGORY('13_Dowel_Pin_ISO_8734_8x16',
'13_Dowel_Pin_ISO_8734_8x16',(#46533));
#46516=APPLICATION_PROTOCOL_DEFINITION('international standard',
'automotive_design',2009,#46517);
#46517=APPLICATION_CONTEXT(
'Core Data for Automotive Mechanical Design Process');
#46518=PRODUCT_CONTEXT('part definition',#46517,'mechanical');
#46519=PRODUCT('2026-10-26-00-50-37-162','MAS-346',$,(#46518));
#46520=PRODUCT('2026-10-26-00-50-38-164','01_Front_Flange_SAE_A',$,(#46518));
#46521=PRODUCT('2026-10-26-00-50-40-883','02_Gear_Body',$,(#46518));
#46522=PRODUCT('2026-10-26-00-50-44-377','03_Rear_Cover',$,(#46518));
#46523=PRODUCT('2026-10-26-00-50-47-232',
'04_Drive_Gear_Shaft_z12_m2.75',$,(#46518));
#46524=PRODUCT('2026-10-26-00-50-58-441',
'05_Driven_Gear_Shaft_z12_m2.75',$,(#46518));
#46525=PRODUCT('2026-10-26-00-51-10-414','06_Bearing_Block_Bronze',$,(#46518));
#46526=PRODUCT('2026-10-26-00-51-13-026','08_Shaft_Lip_Seal_5-8x1-1-8',
$,(#46518));
#46527=PRODUCT('2026-10-26-00-51-13-699','09_Circlip_DIN_472_-_28',$,(#46518));
#46528=PRODUCT('2026-10-26-00-51-14-660','10_Shaft_Key_5-32',$,(#46518));
#46529=PRODUCT('2026-10-26-00-51-15-440','11_Body_Face_Seal_O-Ring',$,(#46518));
#46530=PRODUCT('2026-10-26-00-51-20-172','14_Case_Drain_Plug_9-16-18',$,
(#46518));
#46531=PRODUCT('2026-10-26-00-51-12-008',
'07_Needle_Bearing_HK1716_Drawn_Cup',$,(#46518));
#46532=PRODUCT('2026-10-26-00-51-16-707',
'12_Through_Bolt_ISO_4762_M10x90',$,(#46518));
#46533=PRODUCT('2026-10-26-00-51-19-479','13_Dowel_Pin_ISO_8734_8x16',$,
(#46518));
#46534=PRESENTATION_STYLE_ASSIGNMENT((#46539));
#46535=PRESENTATION_STYLE_ASSIGNMENT((#46540));
#46536=PRESENTATION_STYLE_ASSIGNMENT((#46541));
#46537=PRESENTATION_STYLE_ASSIGNMENT((#46542));
#46538=PRESENTATION_STYLE_ASSIGNMENT((#46543));
#46539=SURFACE_STYLE_USAGE(.BOTH.,#46544);
#46540=SURFACE_STYLE_USAGE(.BOTH.,#46545);
#46541=SURFACE_STYLE_USAGE(.BOTH.,#46546);
#46542=SURFACE_STYLE_USAGE(.BOTH.,#46547);
#46543=SURFACE_STYLE_USAGE(.BOTH.,#46548);
#46544=SURFACE_SIDE_STYLE('',(#46549));
#46545=SURFACE_SIDE_STYLE('',(#46550));
#46546=SURFACE_SIDE_STYLE('',(#46551));
#46547=SURFACE_SIDE_STYLE('',(#46552));
#46548=SURFACE_SIDE_STYLE('',(#46553));
#46549=SURFACE_STYLE_FILL_AREA(#46554);
#46550=SURFACE_STYLE_FILL_AREA(#46555);
#46551=SURFACE_STYLE_FILL_AREA(#46556);
#46552=SURFACE_STYLE_FILL_AREA(#46557);
#46553=SURFACE_STYLE_FILL_AREA(#46558);
#46554=FILL_AREA_STYLE('Steel - Satin',(#46559));
#46555=FILL_AREA_STYLE('MAS496_gun',(#46560));
#46556=FILL_AREA_STYLE('MAS496_al',(#46561));
#46557=FILL_AREA_STYLE('MAS496_ss',(#46562));
#46558=FILL_AREA_STYLE('MAS496_ti',(#46563));
#46559=FILL_AREA_STYLE_COLOUR('Steel - Satin',#46564);
#46560=FILL_AREA_STYLE_COLOUR('MAS496_gun',#46565);
#46561=FILL_AREA_STYLE_COLOUR('MAS496_al',#46566);
#46562=FILL_AREA_STYLE_COLOUR('MAS496_ss',#46567);
#46563=FILL_AREA_STYLE_COLOUR('MAS496_ti',#46568);
#46564=COLOUR_RGB('Steel - Satin',0.627450980392157,0.627450980392157,0.627450980392157);
#46565=COLOUR_RGB('MAS496_gun',0.313725490196078,0.337254901960784,0.364705882352941);
#46566=COLOUR_RGB('MAS496_al',0.67843137254902,0.705882352941177,0.729411764705882);
#46567=COLOUR_RGB('MAS496_ss',0.83921568627451,0.850980392156863,0.862745098039216);
#46568=COLOUR_RGB('MAS496_ti',0.549019607843137,0.572549019607843,0.596078431372549);
#46569=COLOUR_RGB('Dark Blue',0.08,0.2,0.34);
#46570=FILL_AREA_STYLE_COLOUR('',#46569);
#46571=FILL_AREA_STYLE('',(#46570));
#46572=SURFACE_STYLE_FILL_AREA(#46571);
#46573=SURFACE_SIDE_STYLE('',(#46572));
#46574=SURFACE_STYLE_USAGE(.BOTH.,#46573);
#46575=PRESENTATION_STYLE_ASSIGNMENT((#46574));
#46576=COLOUR_RGB('Light Blue',0.38,0.62,0.78);
#46577=FILL_AREA_STYLE_COLOUR('',#46576);
#46578=FILL_AREA_STYLE('',(#46577));
#46579=SURFACE_STYLE_FILL_AREA(#46578);
#46580=SURFACE_SIDE_STYLE('',(#46579));
#46581=SURFACE_STYLE_USAGE(.BOTH.,#46580);
#46582=PRESENTATION_STYLE_ASSIGNMENT((#46581));
#46583=COLOUR_RGB('Sky Blue',0.24,0.69,0.87);
#46584=FILL_AREA_STYLE_COLOUR('',#46583);
#46585=FILL_AREA_STYLE('',(#46584));
#46586=SURFACE_STYLE_FILL_AREA(#46585);
#46587=SURFACE_SIDE_STYLE('',(#46586));
#46588=SURFACE_STYLE_USAGE(.BOTH.,#46587);
#46589=PRESENTATION_STYLE_ASSIGNMENT((#46588));
#46590=COLOUR_RGB('Grey',0.48,0.52,0.57);
#46591=FILL_AREA_STYLE_COLOUR('',#46590);
#46592=FILL_AREA_STYLE('',(#46591));
#46593=SURFACE_STYLE_FILL_AREA(#46592);
#46594=SURFACE_SIDE_STYLE('',(#46593));
#46595=SURFACE_STYLE_USAGE(.BOTH.,#46594);
#46596=PRESENTATION_STYLE_ASSIGNMENT((#46595));
#46597=COLOUR_RGB('Black',0.12,0.14,0.17);
#46598=FILL_AREA_STYLE_COLOUR('',#46597);
#46599=FILL_AREA_STYLE('',(#46598));
#46600=SURFACE_STYLE_FILL_AREA(#46599);
#46601=SURFACE_SIDE_STYLE('',(#46600));
#46602=SURFACE_STYLE_USAGE(.BOTH.,#46601);
#46603=PRESENTATION_STYLE_ASSIGNMENT((#46602));
#46604=COLOUR_RGB('Off White',0.89,0.88,0.83);
#46605=FILL_AREA_STYLE_COLOUR('',#46604);
#46606=FILL_AREA_STYLE('',(#46605));
#46607=SURFACE_STYLE_FILL_AREA(#46606);
#46608=SURFACE_SIDE_STYLE('',(#46607));
#46609=SURFACE_STYLE_USAGE(.BOTH.,#46608);
#46610=PRESENTATION_STYLE_ASSIGNMENT((#46609));
ENDSEC;
END-ISO-10303-21;
